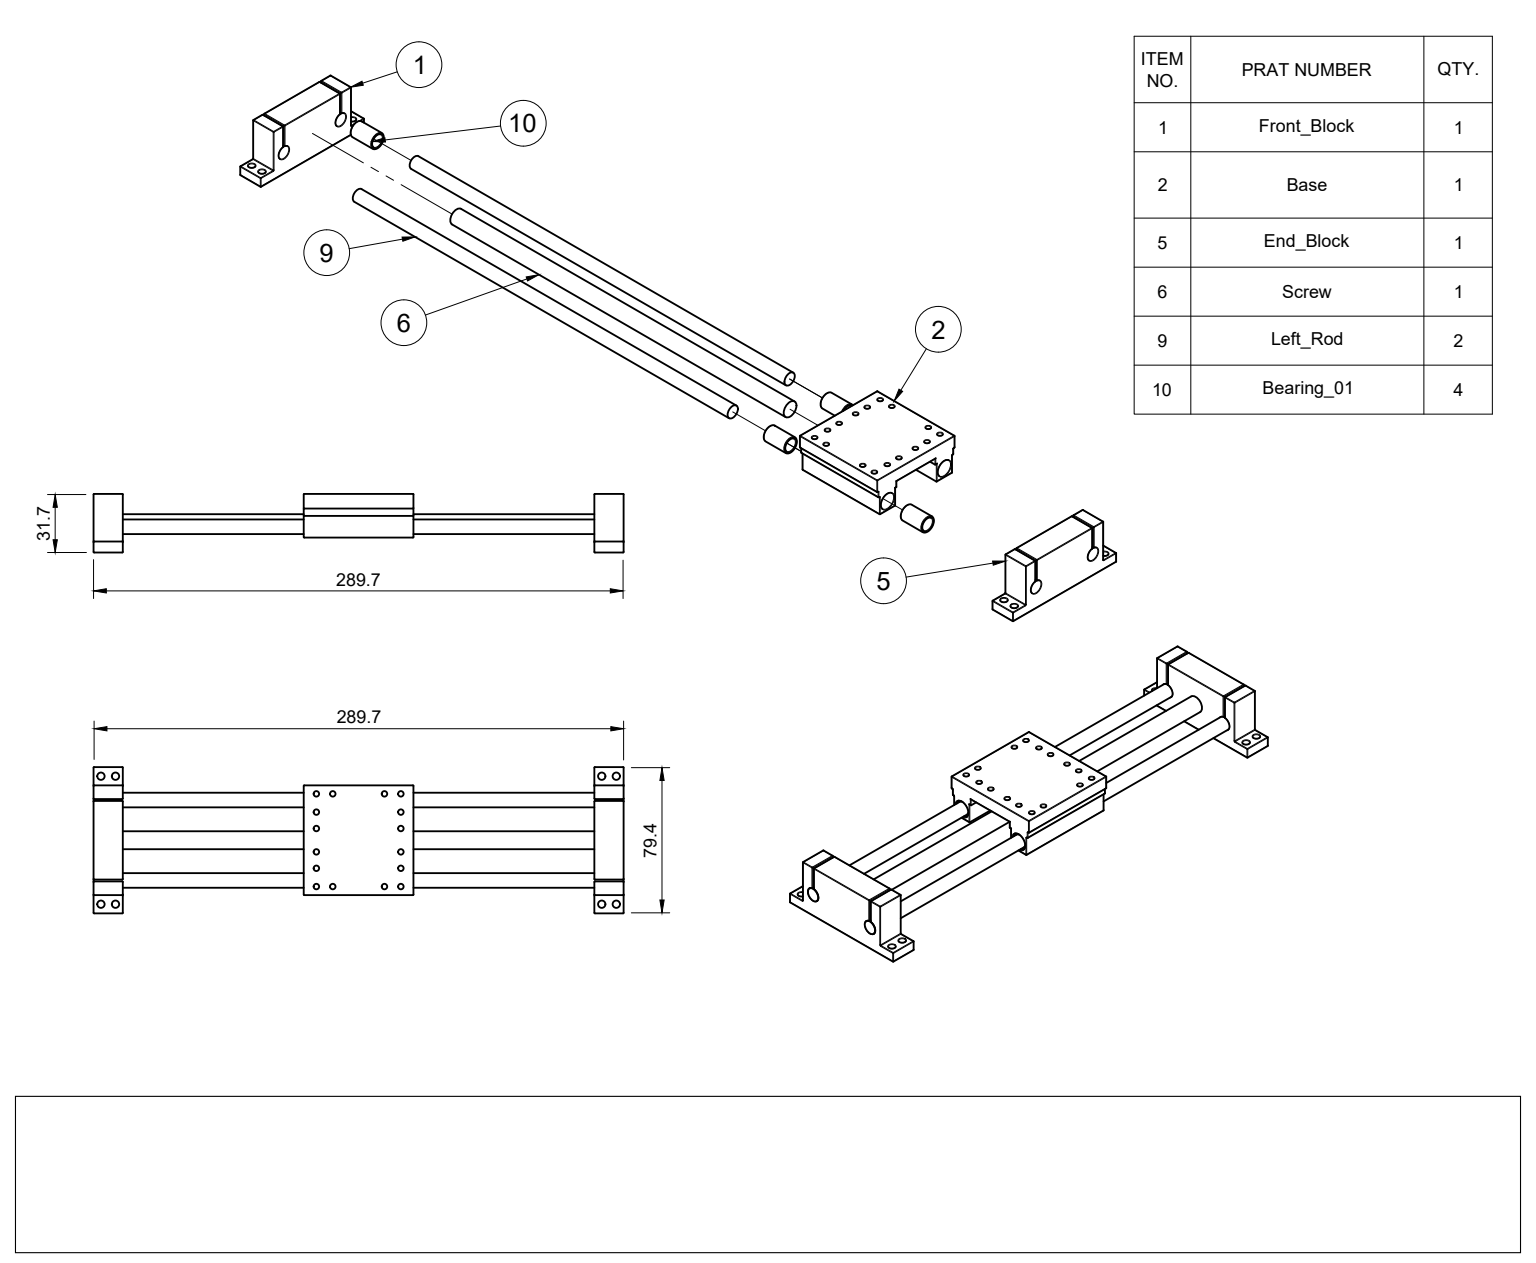
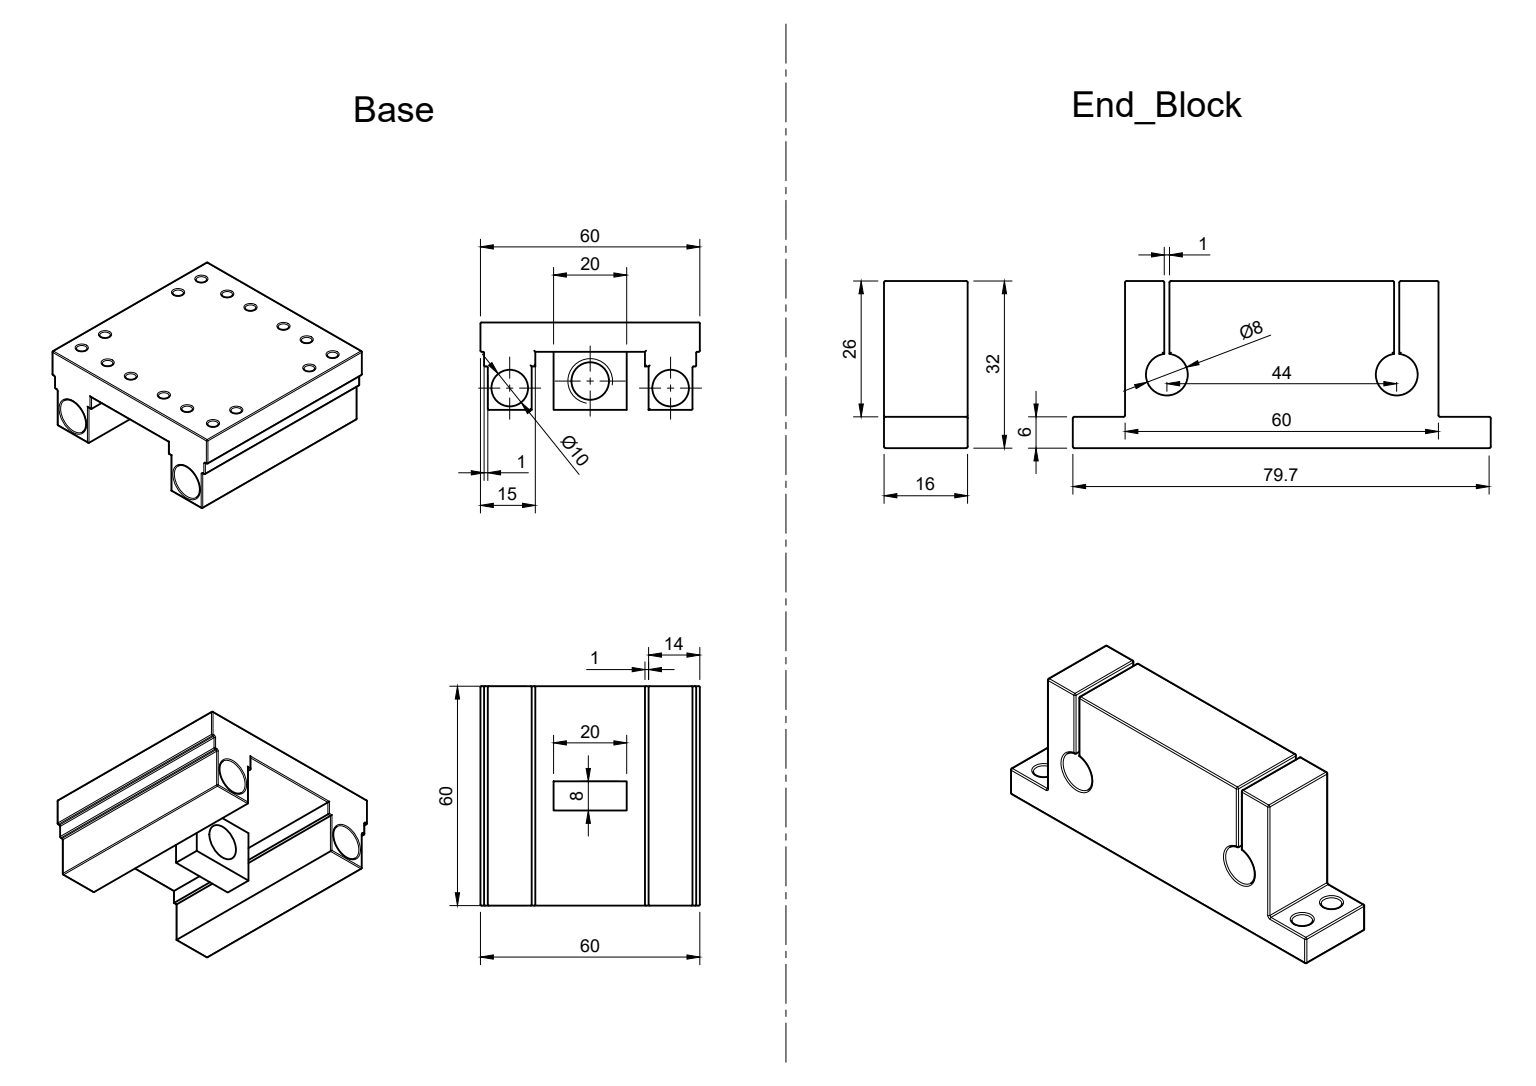
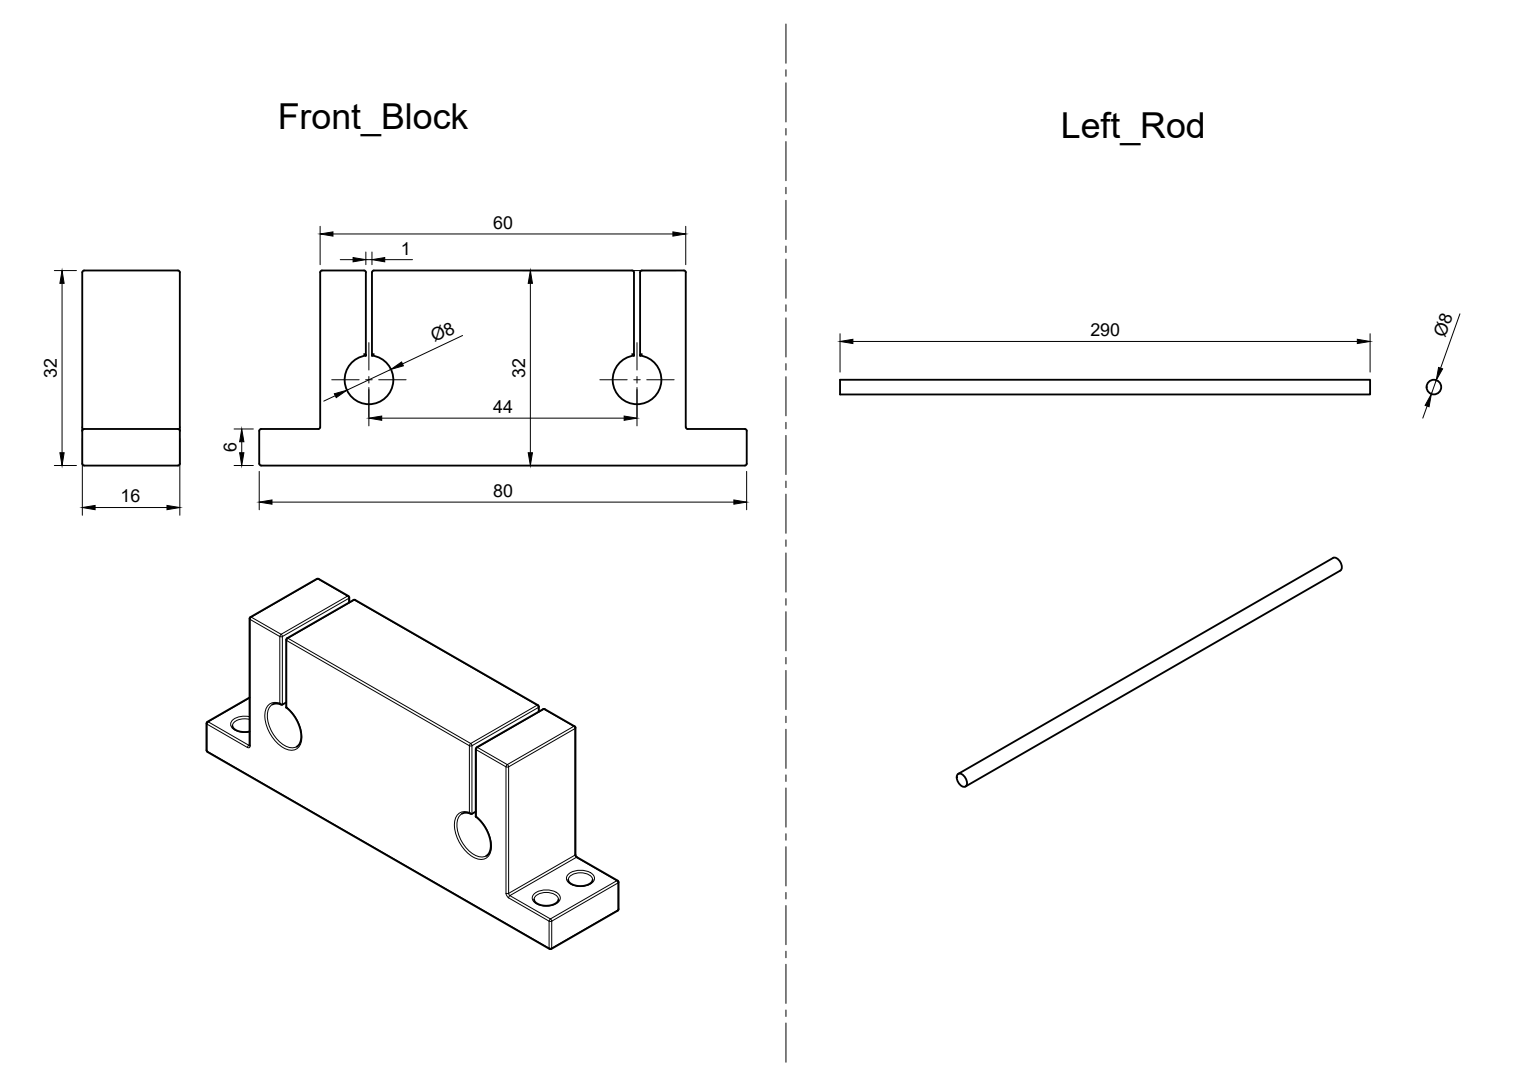
ISO-10303-21;
HEADER;
/* Generated by software containing ST-Developer
 * from STEP Tools, Inc. (www.steptools.com) 
 */

FILE_DESCRIPTION(
/* description */ (''),
/* implementation_level */ '2;1');

FILE_NAME(
/* name */ 'MAS-273',
/* time_stamp */ '2026-10-19T01:30:23+06:00',
/* author */ (''),
/* organization */ (''),
/* preprocessor_version */ 'ST-DEVELOPER v20.2',
/* originating_system */ 'Autodesk Translation Framework v15.15.0.0',
/* authorisation */ '');

FILE_SCHEMA (('AUTOMOTIVE_DESIGN { 1 0 10303 214 3 1 1 }'));
ENDSEC;

DATA;
#10=MECHANICAL_DESIGN_GEOMETRIC_PRESENTATION_REPRESENTATION('',(#87,#88,
#89,#90,#91,#92,#93,#94,#95,#96),#10639);
#11=ITEM_DEFINED_TRANSFORMATION($,$,#5835,#6686);
#12=ITEM_DEFINED_TRANSFORMATION($,$,#6174,#6687);
#13=ITEM_DEFINED_TRANSFORMATION($,$,#6199,#6688);
#14=ITEM_DEFINED_TRANSFORMATION($,$,#6224,#6689);
#15=ITEM_DEFINED_TRANSFORMATION($,$,#6421,#6690);
#16=ITEM_DEFINED_TRANSFORMATION($,$,#6427,#6691);
#17=ITEM_DEFINED_TRANSFORMATION($,$,#6452,#6692);
#18=ITEM_DEFINED_TRANSFORMATION($,$,#6458,#6693);
#19=ITEM_DEFINED_TRANSFORMATION($,$,#6464,#6694);
#20=ITEM_DEFINED_TRANSFORMATION($,$,#6489,#6695);
#21=(
REPRESENTATION_RELATIONSHIP($,$,#10677,#10676)
REPRESENTATION_RELATIONSHIP_WITH_TRANSFORMATION(#11)
SHAPE_REPRESENTATION_RELATIONSHIP()
);
#22=(
REPRESENTATION_RELATIONSHIP($,$,#10678,#10676)
REPRESENTATION_RELATIONSHIP_WITH_TRANSFORMATION(#12)
SHAPE_REPRESENTATION_RELATIONSHIP()
);
#23=(
REPRESENTATION_RELATIONSHIP($,$,#10679,#10676)
REPRESENTATION_RELATIONSHIP_WITH_TRANSFORMATION(#13)
SHAPE_REPRESENTATION_RELATIONSHIP()
);
#24=(
REPRESENTATION_RELATIONSHIP($,$,#10680,#10676)
REPRESENTATION_RELATIONSHIP_WITH_TRANSFORMATION(#14)
SHAPE_REPRESENTATION_RELATIONSHIP()
);
#25=(
REPRESENTATION_RELATIONSHIP($,$,#10681,#10676)
REPRESENTATION_RELATIONSHIP_WITH_TRANSFORMATION(#15)
SHAPE_REPRESENTATION_RELATIONSHIP()
);
#26=(
REPRESENTATION_RELATIONSHIP($,$,#10682,#10676)
REPRESENTATION_RELATIONSHIP_WITH_TRANSFORMATION(#16)
SHAPE_REPRESENTATION_RELATIONSHIP()
);
#27=(
REPRESENTATION_RELATIONSHIP($,$,#10683,#10676)
REPRESENTATION_RELATIONSHIP_WITH_TRANSFORMATION(#17)
SHAPE_REPRESENTATION_RELATIONSHIP()
);
#28=(
REPRESENTATION_RELATIONSHIP($,$,#10684,#10676)
REPRESENTATION_RELATIONSHIP_WITH_TRANSFORMATION(#18)
SHAPE_REPRESENTATION_RELATIONSHIP()
);
#29=(
REPRESENTATION_RELATIONSHIP($,$,#10685,#10676)
REPRESENTATION_RELATIONSHIP_WITH_TRANSFORMATION(#19)
SHAPE_REPRESENTATION_RELATIONSHIP()
);
#30=(
REPRESENTATION_RELATIONSHIP($,$,#10686,#10676)
REPRESENTATION_RELATIONSHIP_WITH_TRANSFORMATION(#20)
SHAPE_REPRESENTATION_RELATIONSHIP()
);
#31=CONTEXT_DEPENDENT_SHAPE_REPRESENTATION(#21,#10666);
#32=CONTEXT_DEPENDENT_SHAPE_REPRESENTATION(#22,#10667);
#33=CONTEXT_DEPENDENT_SHAPE_REPRESENTATION(#23,#10668);
#34=CONTEXT_DEPENDENT_SHAPE_REPRESENTATION(#24,#10669);
#35=CONTEXT_DEPENDENT_SHAPE_REPRESENTATION(#25,#10670);
#36=CONTEXT_DEPENDENT_SHAPE_REPRESENTATION(#26,#10671);
#37=CONTEXT_DEPENDENT_SHAPE_REPRESENTATION(#27,#10672);
#38=CONTEXT_DEPENDENT_SHAPE_REPRESENTATION(#28,#10673);
#39=CONTEXT_DEPENDENT_SHAPE_REPRESENTATION(#29,#10674);
#40=CONTEXT_DEPENDENT_SHAPE_REPRESENTATION(#30,#10675);
#41=NEXT_ASSEMBLY_USAGE_OCCURRENCE('Base:1','Base:1','Base:1',#10688,#10689,
'Base:1');
#42=NEXT_ASSEMBLY_USAGE_OCCURRENCE('Bearing_03:1','Bearing_03:1',
'Bearing_03:1',#10688,#10690,'Bearing_03:1');
#43=NEXT_ASSEMBLY_USAGE_OCCURRENCE('Bearing_04:1','Bearing_04:1',
'Bearing_04:1',#10688,#10691,'Bearing_04:1');
#44=NEXT_ASSEMBLY_USAGE_OCCURRENCE('End_Block:1','End_Block:1',
'End_Block:1',#10688,#10692,'End_Block:1');
#45=NEXT_ASSEMBLY_USAGE_OCCURRENCE('Screw:1','Screw:1','Screw:1',#10688,
#10693,'Screw:1');
#46=NEXT_ASSEMBLY_USAGE_OCCURRENCE('Bearing_02:1','Bearing_02:1',
'Bearing_02:1',#10688,#10694,'Bearing_02:1');
#47=NEXT_ASSEMBLY_USAGE_OCCURRENCE('Left_Rod:1','Left_Rod:1',
'Left_Rod:1',#10688,#10695,'Left_Rod:1');
#48=NEXT_ASSEMBLY_USAGE_OCCURRENCE('Right_Rod:1','Right_Rod:1',
'Right_Rod:1',#10688,#10696,'Right_Rod:1');
#49=NEXT_ASSEMBLY_USAGE_OCCURRENCE('Bearing_01:1','Bearing_01:1',
'Bearing_01:1',#10688,#10697,'Bearing_01:1');
#50=NEXT_ASSEMBLY_USAGE_OCCURRENCE('Front_Block:1','Front_Block:1',
'Front_Block:1',#10688,#10698,'Front_Block:1');
#51=B_SPLINE_CURVE_WITH_KNOTS('',3,(#9730,#9731,#9732,#9733,#9734,#9735,
#9736,#9737,#9738,#9739,#9740,#9741,#9742,#9743),.UNSPECIFIED.,.F.,.F.,
(4,2,2,2,2,2,4),(-0.0546723895048706,-0.0456918425711812,-0.0355825901397237,
-0.0226053755936092,-0.0114630731161328,0.,0.000317608874346033),
 .UNSPECIFIED.);
#52=B_SPLINE_CURVE_WITH_KNOTS('',3,(#9762,#9763,#9764,#9765,#9766,#9767,
#9768,#9769,#9770,#9771,#9772,#9773,#9774,#9775),.UNSPECIFIED.,.F.,.F.,
(4,2,2,2,2,2,4),(-0.0545709206888463,-0.0542557323018554,-0.0428800190516867,
-0.0318226318386046,-0.0189443163854003,-0.00891210636484469,0.),
 .UNSPECIFIED.);
#53=B_SPLINE_CURVE_WITH_KNOTS('',3,(#9781,#9782,#9783,#9784,#9785,#9786,
#9787,#9788,#9789,#9790,#9791,#9792,#9793,#9794),.UNSPECIFIED.,.F.,.F.,
(4,2,2,2,2,2,4),(-0.054570920688858,-0.0542557323018634,-0.0428800190517046,
-0.0318226318386095,-0.0189443163853947,-0.00891210636484256,0.),
 .UNSPECIFIED.);
#54=B_SPLINE_CURVE_WITH_KNOTS('',3,(#9800,#9801,#9802,#9803,#9804,#9805,
#9806,#9807,#9808,#9809,#9810,#9811,#9812,#9813),.UNSPECIFIED.,.F.,.F.,
(4,2,2,2,2,2,4),(-0.0546723899568943,-0.0456918429465685,-0.035582590428848,
-0.0226053757720057,-0.0114630731991726,0.,0.000317608880617367),
 .UNSPECIFIED.);
#55=B_SPLINE_CURVE_WITH_KNOTS('',3,(#9850,#9851,#9852,#9853,#9854,#9855,
#9856,#9857,#9858,#9859,#9860,#9861,#9862,#9863),.UNSPECIFIED.,.F.,.F.,
(4,2,2,2,2,2,4),(-0.0545709206888251,-0.0542557323018344,-0.0428800190516725,
-0.031822631838589,-0.0189443163853906,-0.00891210636484253,0.),
 .UNSPECIFIED.);
#56=B_SPLINE_CURVE_WITH_KNOTS('',3,(#9875,#9876,#9877,#9878,#9879,#9880,
#9881,#9882,#9883,#9884,#9885,#9886,#9887,#9888),.UNSPECIFIED.,.F.,.F.,
(4,2,2,2,2,2,4),(-0.0546723899569042,-0.0456918429465809,-0.0355825904288576,
-0.0226053757720114,-0.0114630731991751,0.,0.000317608880617457),
 .UNSPECIFIED.);
#57=B_SPLINE_CURVE_WITH_KNOTS('',3,(#9897,#9898,#9899,#9900,#9901,#9902,
#9903,#9904,#9905,#9906,#9907,#9908,#9909,#9910),.UNSPECIFIED.,.F.,.F.,
(4,2,2,2,2,2,4),(-0.0546723899569031,-0.0456918429465823,-0.0355825904288603,
-0.0226053757720111,-0.0114630731991739,0.,0.000317608880617373),
 .UNSPECIFIED.);
#58=B_SPLINE_CURVE_WITH_KNOTS('',3,(#9919,#9920,#9921,#9922,#9923,#9924,
#9925,#9926,#9927,#9928,#9929,#9930,#9931,#9932),.UNSPECIFIED.,.F.,.F.,
(4,2,2,2,2,2,4),(-0.0545709206996626,-0.0542557323162056,-0.0428800190513851,
-0.0318226318385961,-0.0189443163854002,-0.00891210636484565,0.),
 .UNSPECIFIED.);
#59=B_SPLINE_CURVE_WITH_KNOTS('',3,(#10339,#10340,#10341,#10342,#10343,
#10344,#10345,#10346,#10347,#10348,#10349,#10350,#10351,#10352),
 .UNSPECIFIED.,.F.,.F.,(4,2,2,2,2,2,4),(-0.0546723895048706,-0.0456918425711812,
-0.0355825901397237,-0.0226053755936092,-0.0114630731161328,0.,0.000317608874346033),
 .UNSPECIFIED.);
#60=B_SPLINE_CURVE_WITH_KNOTS('',3,(#10371,#10372,#10373,#10374,#10375,
#10376,#10377,#10378,#10379,#10380,#10381,#10382,#10383,#10384),
 .UNSPECIFIED.,.F.,.F.,(4,2,2,2,2,2,4),(-0.0545709206888463,-0.0542557323018554,
-0.0428800190516867,-0.0318226318386046,-0.0189443163854003,-0.00891210636484469,
0.),.UNSPECIFIED.);
#61=B_SPLINE_CURVE_WITH_KNOTS('',3,(#10390,#10391,#10392,#10393,#10394,
#10395,#10396,#10397,#10398,#10399,#10400,#10401,#10402,#10403),
 .UNSPECIFIED.,.F.,.F.,(4,2,2,2,2,2,4),(-0.054570920688858,-0.0542557323018634,
-0.0428800190517046,-0.0318226318386095,-0.0189443163853947,-0.00891210636484256,
0.),.UNSPECIFIED.);
#62=B_SPLINE_CURVE_WITH_KNOTS('',3,(#10409,#10410,#10411,#10412,#10413,
#10414,#10415,#10416,#10417,#10418,#10419,#10420,#10421,#10422),
 .UNSPECIFIED.,.F.,.F.,(4,2,2,2,2,2,4),(-0.0546723899568943,-0.0456918429465685,
-0.035582590428848,-0.0226053757720057,-0.0114630731991726,0.,0.000317608880617367),
 .UNSPECIFIED.);
#63=B_SPLINE_CURVE_WITH_KNOTS('',3,(#10459,#10460,#10461,#10462,#10463,
#10464,#10465,#10466,#10467,#10468,#10469,#10470,#10471,#10472),
 .UNSPECIFIED.,.F.,.F.,(4,2,2,2,2,2,4),(-0.0545709206888251,-0.0542557323018344,
-0.0428800190516725,-0.031822631838589,-0.0189443163853906,-0.00891210636484253,
0.),.UNSPECIFIED.);
#64=B_SPLINE_CURVE_WITH_KNOTS('',3,(#10484,#10485,#10486,#10487,#10488,
#10489,#10490,#10491,#10492,#10493,#10494,#10495,#10496,#10497),
 .UNSPECIFIED.,.F.,.F.,(4,2,2,2,2,2,4),(-0.0546723899569042,-0.0456918429465809,
-0.0355825904288576,-0.0226053757720114,-0.0114630731991751,0.,0.000317608880617457),
 .UNSPECIFIED.);
#65=B_SPLINE_CURVE_WITH_KNOTS('',3,(#10506,#10507,#10508,#10509,#10510,
#10511,#10512,#10513,#10514,#10515,#10516,#10517,#10518,#10519),
 .UNSPECIFIED.,.F.,.F.,(4,2,2,2,2,2,4),(-0.0546723899569031,-0.0456918429465823,
-0.0355825904288603,-0.0226053757720111,-0.0114630731991739,0.,0.000317608880617373),
 .UNSPECIFIED.);
#66=B_SPLINE_CURVE_WITH_KNOTS('',3,(#10528,#10529,#10530,#10531,#10532,
#10533,#10534,#10535,#10536,#10537,#10538,#10539,#10540,#10541),
 .UNSPECIFIED.,.F.,.F.,(4,2,2,2,2,2,4),(-0.0545709206996626,-0.0542557323162056,
-0.0428800190513851,-0.0318226318385961,-0.0189443163854002,-0.00891210636484565,
0.),.UNSPECIFIED.);
#67=SHAPE_REPRESENTATION_RELATIONSHIP('SRR','None',#10677,#77);
#68=SHAPE_REPRESENTATION_RELATIONSHIP('SRR','None',#10678,#78);
#69=SHAPE_REPRESENTATION_RELATIONSHIP('SRR','None',#10679,#79);
#70=SHAPE_REPRESENTATION_RELATIONSHIP('SRR','None',#10680,#80);
#71=SHAPE_REPRESENTATION_RELATIONSHIP('SRR','None',#10681,#81);
#72=SHAPE_REPRESENTATION_RELATIONSHIP('SRR','None',#10682,#82);
#73=SHAPE_REPRESENTATION_RELATIONSHIP('SRR','None',#10683,#83);
#74=SHAPE_REPRESENTATION_RELATIONSHIP('SRR','None',#10684,#84);
#75=SHAPE_REPRESENTATION_RELATIONSHIP('SRR','None',#10685,#85);
#76=SHAPE_REPRESENTATION_RELATIONSHIP('SRR','None',#10686,#86);
#77=ADVANCED_BREP_SHAPE_REPRESENTATION('',(#97),#10629);
#78=ADVANCED_BREP_SHAPE_REPRESENTATION('',(#98),#10630);
#79=ADVANCED_BREP_SHAPE_REPRESENTATION('',(#99),#10631);
#80=ADVANCED_BREP_SHAPE_REPRESENTATION('',(#100),#10632);
#81=ADVANCED_BREP_SHAPE_REPRESENTATION('',(#101),#10633);
#82=ADVANCED_BREP_SHAPE_REPRESENTATION('',(#102),#10634);
#83=ADVANCED_BREP_SHAPE_REPRESENTATION('',(#103),#10635);
#84=ADVANCED_BREP_SHAPE_REPRESENTATION('',(#104),#10636);
#85=ADVANCED_BREP_SHAPE_REPRESENTATION('',(#105),#10637);
#86=ADVANCED_BREP_SHAPE_REPRESENTATION('',(#106),#10638);
#87=STYLED_ITEM('',(#10769),#97);
#88=STYLED_ITEM('',(#10790),#98);
#89=STYLED_ITEM('',(#10790),#99);
#90=STYLED_ITEM('',(#10769),#100);
#91=STYLED_ITEM('',(#10797),#101);
#92=STYLED_ITEM('',(#10790),#102);
#93=STYLED_ITEM('',(#10790),#103);
#94=STYLED_ITEM('',(#10790),#104);
#95=STYLED_ITEM('',(#10790),#105);
#96=STYLED_ITEM('',(#10769),#106);
#97=MANIFOLD_SOLID_BREP('Base',#5713);
#98=MANIFOLD_SOLID_BREP('Bearing_03',#5714);
#99=MANIFOLD_SOLID_BREP('Bearing_04',#5715);
#100=MANIFOLD_SOLID_BREP('End_Block',#5716);
#101=MANIFOLD_SOLID_BREP('Screw',#5717);
#102=MANIFOLD_SOLID_BREP('Bearing_02',#5718);
#103=MANIFOLD_SOLID_BREP('Left_Rod',#5719);
#104=MANIFOLD_SOLID_BREP('Right_Rod',#5720);
#105=MANIFOLD_SOLID_BREP('Bearing_01',#5721);
#106=MANIFOLD_SOLID_BREP('Front_Block',#5722);
#107=SPHERICAL_SURFACE('',#5994,0.299999999999998);
#108=SPHERICAL_SURFACE('',#5998,0.3);
#109=SPHERICAL_SURFACE('',#6004,0.299999999999998);
#110=SPHERICAL_SURFACE('',#6014,0.3);
#111=SPHERICAL_SURFACE('',#6030,0.299999999999998);
#112=SPHERICAL_SURFACE('',#6038,0.3);
#113=SPHERICAL_SURFACE('',#6044,0.3);
#114=SPHERICAL_SURFACE('',#6052,0.299999999999994);
#115=SPHERICAL_SURFACE('',#6067,0.299999999999998);
#116=SPHERICAL_SURFACE('',#6075,0.3);
#117=SPHERICAL_SURFACE('',#6081,0.3);
#118=SPHERICAL_SURFACE('',#6085,0.3);
#119=SPHERICAL_SURFACE('',#6089,0.299999999999998);
#120=SPHERICAL_SURFACE('',#6094,0.299999999999998);
#121=SPHERICAL_SURFACE('',#6100,0.299999999999998);
#122=SPHERICAL_SURFACE('',#6104,0.300000000000002);
#123=SPHERICAL_SURFACE('',#6253,0.3);
#124=SPHERICAL_SURFACE('',#6257,0.299999999999994);
#125=SPHERICAL_SURFACE('',#6261,0.300000000000011);
#126=SPHERICAL_SURFACE('',#6266,0.299999999999998);
#127=SPHERICAL_SURFACE('',#6271,0.3);
#128=SPHERICAL_SURFACE('',#6277,0.299999999999994);
#129=SPHERICAL_SURFACE('',#6282,0.3);
#130=SPHERICAL_SURFACE('',#6291,0.3);
#131=SPHERICAL_SURFACE('',#6306,0.299999999999998);
#132=SPHERICAL_SURFACE('',#6316,0.299999999999994);
#133=SPHERICAL_SURFACE('',#6321,0.299999999999994);
#134=SPHERICAL_SURFACE('',#6326,0.3);
#135=SPHERICAL_SURFACE('',#6331,0.299999999999994);
#136=SPHERICAL_SURFACE('',#6337,0.299999999999998);
#137=SPHERICAL_SURFACE('',#6341,0.300000000000002);
#138=SPHERICAL_SURFACE('',#6346,0.3);
#139=SPHERICAL_SURFACE('',#6355,0.3);
#140=SPHERICAL_SURFACE('',#6359,0.3);
#141=SPHERICAL_SURFACE('',#6363,0.3);
#142=SPHERICAL_SURFACE('',#6368,0.299999999999994);
#143=SPHERICAL_SURFACE('',#6518,0.3);
#144=SPHERICAL_SURFACE('',#6522,0.299999999999994);
#145=SPHERICAL_SURFACE('',#6526,0.300000000000011);
#146=SPHERICAL_SURFACE('',#6531,0.299999999999998);
#147=SPHERICAL_SURFACE('',#6536,0.3);
#148=SPHERICAL_SURFACE('',#6542,0.299999999999994);
#149=SPHERICAL_SURFACE('',#6547,0.3);
#150=SPHERICAL_SURFACE('',#6556,0.3);
#151=SPHERICAL_SURFACE('',#6571,0.299999999999998);
#152=SPHERICAL_SURFACE('',#6581,0.299999999999994);
#153=SPHERICAL_SURFACE('',#6586,0.299999999999994);
#154=SPHERICAL_SURFACE('',#6591,0.3);
#155=SPHERICAL_SURFACE('',#6596,0.299999999999994);
#156=SPHERICAL_SURFACE('',#6602,0.299999999999998);
#157=SPHERICAL_SURFACE('',#6606,0.300000000000002);
#158=SPHERICAL_SURFACE('',#6611,0.3);
#159=SPHERICAL_SURFACE('',#6620,0.3);
#160=SPHERICAL_SURFACE('',#6624,0.3);
#161=SPHERICAL_SURFACE('',#6628,0.3);
#162=SPHERICAL_SURFACE('',#6633,0.299999999999994);
#163=ELLIPSE('',#5976,0.42426406871193,0.3);
#164=ELLIPSE('',#5977,0.424264068711927,0.3);
#165=ELLIPSE('',#5979,0.42426406871193,0.3);
#166=ELLIPSE('',#5980,0.424264068711927,0.3);
#167=ELLIPSE('',#5982,0.424264068711929,0.3);
#168=ELLIPSE('',#5984,0.424264068711929,0.3);
#169=ELLIPSE('',#5986,0.424264068711929,0.3);
#170=ELLIPSE('',#5988,0.424264068711929,0.3);
#171=ELLIPSE('',#5990,0.424264068711929,0.3);
#172=ELLIPSE('',#5991,0.424264068711929,0.3);
#173=ELLIPSE('',#5993,0.424264068711929,0.3);
#174=ELLIPSE('',#6009,0.424264068711929,0.3);
#175=ELLIPSE('',#6019,0.424264068711929,0.3);
#176=ELLIPSE('',#6131,0.424264068711929,0.3);
#177=ELLIPSE('',#6134,0.424264068711929,0.3);
#178=ELLIPSE('',#6137,0.424264068711929,0.3);
#179=TOROIDAL_SURFACE('',#5844,5.3,0.3);
#180=TOROIDAL_SURFACE('',#5858,5.3,0.3);
#181=TOROIDAL_SURFACE('',#5865,5.3,0.3);
#182=TOROIDAL_SURFACE('',#5874,5.3,0.3);
#183=TOROIDAL_SURFACE('',#5876,1.8,0.3);
#184=TOROIDAL_SURFACE('',#5898,1.8,0.3);
#185=TOROIDAL_SURFACE('',#5903,1.8,0.3);
#186=TOROIDAL_SURFACE('',#5908,1.8,0.3);
#187=TOROIDAL_SURFACE('',#5913,1.8,0.3);
#188=TOROIDAL_SURFACE('',#5918,1.8,0.3);
#189=TOROIDAL_SURFACE('',#5923,1.8,0.3);
#190=TOROIDAL_SURFACE('',#5928,1.8,0.3);
#191=TOROIDAL_SURFACE('',#5934,1.8,0.3);
#192=TOROIDAL_SURFACE('',#5939,1.8,0.3);
#193=TOROIDAL_SURFACE('',#5945,1.8,0.3);
#194=TOROIDAL_SURFACE('',#5950,1.8,0.3);
#195=TOROIDAL_SURFACE('',#5955,1.8,0.3);
#196=TOROIDAL_SURFACE('',#5960,1.8,0.3);
#197=TOROIDAL_SURFACE('',#5965,1.8,0.3);
#198=TOROIDAL_SURFACE('',#5970,1.8,0.3);
#199=TOROIDAL_SURFACE('',#6010,0.599999999999996,0.299999999999998);
#200=TOROIDAL_SURFACE('',#6021,0.600000000000001,0.3);
#201=TOROIDAL_SURFACE('',#6026,0.599999999999996,0.299999999999998);
#202=TOROIDAL_SURFACE('',#6034,0.599999999999996,0.299999999999998);
#203=TOROIDAL_SURFACE('',#6048,0.600000000000001,0.299999999999998);
#204=TOROIDAL_SURFACE('',#6057,0.600000000000001,0.3);
#205=TOROIDAL_SURFACE('',#6062,0.600000000000001,0.3);
#206=TOROIDAL_SURFACE('',#6071,0.599999999999996,0.299999999999998);
#207=TOROIDAL_SURFACE('',#6175,4.3,0.3);
#208=TOROIDAL_SURFACE('',#6185,4.7,0.3);
#209=TOROIDAL_SURFACE('',#6192,4.3,0.3);
#210=TOROIDAL_SURFACE('',#6197,4.7,0.3);
#211=TOROIDAL_SURFACE('',#6200,4.3,0.3);
#212=TOROIDAL_SURFACE('',#6210,4.7,0.3);
#213=TOROIDAL_SURFACE('',#6217,4.3,0.3);
#214=TOROIDAL_SURFACE('',#6222,4.7,0.3);
#215=TOROIDAL_SURFACE('',#6225,2.29999999999999,0.3);
#216=TOROIDAL_SURFACE('',#6233,2.29999999999999,0.3);
#217=TOROIDAL_SURFACE('',#6238,2.29999999999999,0.3);
#218=TOROIDAL_SURFACE('',#6247,2.29999999999999,0.3);
#219=TOROIDAL_SURFACE('',#6286,0.600000000000001,0.3);
#220=TOROIDAL_SURFACE('',#6296,0.600000000000001,0.299999999999994);
#221=TOROIDAL_SURFACE('',#6301,0.600000000000001,0.299999999999976);
#222=TOROIDAL_SURFACE('',#6311,0.600000000000001,0.3);
#223=TOROIDAL_SURFACE('',#6378,4.3,0.3);
#224=TOROIDAL_SURFACE('',#6382,4.3,0.3);
#225=TOROIDAL_SURFACE('',#6385,4.3,0.3);
#226=TOROIDAL_SURFACE('',#6388,4.3,0.3);
#227=TOROIDAL_SURFACE('',#6428,4.3,0.3);
#228=TOROIDAL_SURFACE('',#6438,4.7,0.3);
#229=TOROIDAL_SURFACE('',#6445,4.3,0.3);
#230=TOROIDAL_SURFACE('',#6450,4.7,0.3);
#231=TOROIDAL_SURFACE('',#6465,4.3,0.3);
#232=TOROIDAL_SURFACE('',#6475,4.7,0.3);
#233=TOROIDAL_SURFACE('',#6482,4.3,0.3);
#234=TOROIDAL_SURFACE('',#6487,4.7,0.3);
#235=TOROIDAL_SURFACE('',#6490,2.29999999999999,0.3);
#236=TOROIDAL_SURFACE('',#6498,2.29999999999999,0.3);
#237=TOROIDAL_SURFACE('',#6503,2.29999999999999,0.3);
#238=TOROIDAL_SURFACE('',#6512,2.29999999999999,0.3);
#239=TOROIDAL_SURFACE('',#6551,0.600000000000001,0.3);
#240=TOROIDAL_SURFACE('',#6561,0.600000000000001,0.299999999999994);
#241=TOROIDAL_SURFACE('',#6566,0.600000000000001,0.299999999999976);
#242=TOROIDAL_SURFACE('',#6576,0.600000000000001,0.3);
#243=TOROIDAL_SURFACE('',#6643,4.3,0.3);
#244=TOROIDAL_SURFACE('',#6647,4.3,0.3);
#245=TOROIDAL_SURFACE('',#6650,4.3,0.3);
#246=TOROIDAL_SURFACE('',#6653,4.3,0.3);
#247=FACE_BOUND('',#773,.T.);
#248=FACE_BOUND('',#776,.T.);
#249=FACE_BOUND('',#780,.T.);
#250=FACE_BOUND('',#781,.T.);
#251=FACE_BOUND('',#787,.T.);
#252=FACE_BOUND('',#788,.T.);
#253=FACE_BOUND('',#792,.T.);
#254=FACE_BOUND('',#793,.T.);
#255=FACE_BOUND('',#794,.T.);
#256=FACE_BOUND('',#795,.T.);
#257=FACE_BOUND('',#796,.T.);
#258=FACE_BOUND('',#797,.T.);
#259=FACE_BOUND('',#798,.T.);
#260=FACE_BOUND('',#799,.T.);
#261=FACE_BOUND('',#800,.T.);
#262=FACE_BOUND('',#801,.T.);
#263=FACE_BOUND('',#802,.T.);
#264=FACE_BOUND('',#803,.T.);
#265=FACE_BOUND('',#804,.T.);
#266=FACE_BOUND('',#805,.T.);
#267=FACE_BOUND('',#806,.T.);
#268=FACE_BOUND('',#807,.T.);
#269=FACE_BOUND('',#919,.T.);
#270=FACE_BOUND('',#953,.T.);
#271=FACE_BOUND('',#959,.T.);
#272=FACE_BOUND('',#963,.T.);
#273=FACE_BOUND('',#969,.T.);
#274=FACE_BOUND('',#973,.T.);
#275=FACE_BOUND('',#974,.T.);
#276=FACE_BOUND('',#980,.T.);
#277=FACE_BOUND('',#981,.T.);
#278=FACE_BOUND('',#1058,.T.);
#279=FACE_BOUND('',#1059,.T.);
#280=FACE_BOUND('',#1060,.T.);
#281=FACE_BOUND('',#1061,.T.);
#282=FACE_BOUND('',#1078,.T.);
#283=FACE_BOUND('',#1084,.T.);
#284=FACE_BOUND('',#1094,.T.);
#285=FACE_BOUND('',#1100,.T.);
#286=FACE_BOUND('',#1104,.T.);
#287=FACE_BOUND('',#1105,.T.);
#288=FACE_BOUND('',#1111,.T.);
#289=FACE_BOUND('',#1112,.T.);
#290=FACE_BOUND('',#1189,.T.);
#291=FACE_BOUND('',#1190,.T.);
#292=FACE_BOUND('',#1191,.T.);
#293=FACE_BOUND('',#1192,.T.);
#294=PLANE('',#5839);
#295=PLANE('',#5840);
#296=PLANE('',#5841);
#297=PLANE('',#5842);
#298=PLANE('',#5843);
#299=PLANE('',#5849);
#300=PLANE('',#5868);
#301=PLANE('',#5880);
#302=PLANE('',#6139);
#303=PLANE('',#6140);
#304=PLANE('',#6141);
#305=PLANE('',#6142);
#306=PLANE('',#6143);
#307=PLANE('',#6144);
#308=PLANE('',#6145);
#309=PLANE('',#6146);
#310=PLANE('',#6147);
#311=PLANE('',#6148);
#312=PLANE('',#6149);
#313=PLANE('',#6150);
#314=PLANE('',#6151);
#315=PLANE('',#6152);
#316=PLANE('',#6153);
#317=PLANE('',#6154);
#318=PLANE('',#6155);
#319=PLANE('',#6156);
#320=PLANE('',#6157);
#321=PLANE('',#6158);
#322=PLANE('',#6159);
#323=PLANE('',#6160);
#324=PLANE('',#6161);
#325=PLANE('',#6162);
#326=PLANE('',#6163);
#327=PLANE('',#6164);
#328=PLANE('',#6165);
#329=PLANE('',#6166);
#330=PLANE('',#6167);
#331=PLANE('',#6168);
#332=PLANE('',#6169);
#333=PLANE('',#6170);
#334=PLANE('',#6171);
#335=PLANE('',#6172);
#336=PLANE('',#6173);
#337=PLANE('',#6180);
#338=PLANE('',#6195);
#339=PLANE('',#6205);
#340=PLANE('',#6220);
#341=PLANE('',#6229);
#342=PLANE('',#6243);
#343=PLANE('',#6405);
#344=PLANE('',#6408);
#345=PLANE('',#6409);
#346=PLANE('',#6410);
#347=PLANE('',#6411);
#348=PLANE('',#6412);
#349=PLANE('',#6413);
#350=PLANE('',#6414);
#351=PLANE('',#6415);
#352=PLANE('',#6416);
#353=PLANE('',#6417);
#354=PLANE('',#6418);
#355=PLANE('',#6419);
#356=PLANE('',#6420);
#357=PLANE('',#6422);
#358=PLANE('',#6426);
#359=PLANE('',#6433);
#360=PLANE('',#6448);
#361=PLANE('',#6453);
#362=PLANE('',#6457);
#363=PLANE('',#6459);
#364=PLANE('',#6463);
#365=PLANE('',#6470);
#366=PLANE('',#6485);
#367=PLANE('',#6494);
#368=PLANE('',#6508);
#369=PLANE('',#6670);
#370=PLANE('',#6673);
#371=PLANE('',#6674);
#372=PLANE('',#6675);
#373=PLANE('',#6676);
#374=PLANE('',#6677);
#375=PLANE('',#6678);
#376=PLANE('',#6679);
#377=PLANE('',#6680);
#378=PLANE('',#6681);
#379=PLANE('',#6682);
#380=PLANE('',#6683);
#381=PLANE('',#6684);
#382=PLANE('',#6685);
#383=FACE_OUTER_BOUND('',#770,.T.);
#384=FACE_OUTER_BOUND('',#771,.T.);
#385=FACE_OUTER_BOUND('',#772,.T.);
#386=FACE_OUTER_BOUND('',#774,.T.);
#387=FACE_OUTER_BOUND('',#775,.T.);
#388=FACE_OUTER_BOUND('',#777,.T.);
#389=FACE_OUTER_BOUND('',#778,.T.);
#390=FACE_OUTER_BOUND('',#779,.T.);
#391=FACE_OUTER_BOUND('',#782,.T.);
#392=FACE_OUTER_BOUND('',#783,.T.);
#393=FACE_OUTER_BOUND('',#784,.T.);
#394=FACE_OUTER_BOUND('',#785,.T.);
#395=FACE_OUTER_BOUND('',#786,.T.);
#396=FACE_OUTER_BOUND('',#789,.T.);
#397=FACE_OUTER_BOUND('',#790,.T.);
#398=FACE_OUTER_BOUND('',#791,.T.);
#399=FACE_OUTER_BOUND('',#808,.T.);
#400=FACE_OUTER_BOUND('',#809,.T.);
#401=FACE_OUTER_BOUND('',#810,.T.);
#402=FACE_OUTER_BOUND('',#811,.T.);
#403=FACE_OUTER_BOUND('',#812,.T.);
#404=FACE_OUTER_BOUND('',#813,.T.);
#405=FACE_OUTER_BOUND('',#814,.T.);
#406=FACE_OUTER_BOUND('',#815,.T.);
#407=FACE_OUTER_BOUND('',#816,.T.);
#408=FACE_OUTER_BOUND('',#817,.T.);
#409=FACE_OUTER_BOUND('',#818,.T.);
#410=FACE_OUTER_BOUND('',#819,.T.);
#411=FACE_OUTER_BOUND('',#820,.T.);
#412=FACE_OUTER_BOUND('',#821,.T.);
#413=FACE_OUTER_BOUND('',#822,.T.);
#414=FACE_OUTER_BOUND('',#823,.T.);
#415=FACE_OUTER_BOUND('',#824,.T.);
#416=FACE_OUTER_BOUND('',#825,.T.);
#417=FACE_OUTER_BOUND('',#826,.T.);
#418=FACE_OUTER_BOUND('',#827,.T.);
#419=FACE_OUTER_BOUND('',#828,.T.);
#420=FACE_OUTER_BOUND('',#829,.T.);
#421=FACE_OUTER_BOUND('',#830,.T.);
#422=FACE_OUTER_BOUND('',#831,.T.);
#423=FACE_OUTER_BOUND('',#832,.T.);
#424=FACE_OUTER_BOUND('',#833,.T.);
#425=FACE_OUTER_BOUND('',#834,.T.);
#426=FACE_OUTER_BOUND('',#835,.T.);
#427=FACE_OUTER_BOUND('',#836,.T.);
#428=FACE_OUTER_BOUND('',#837,.T.);
#429=FACE_OUTER_BOUND('',#838,.T.);
#430=FACE_OUTER_BOUND('',#839,.T.);
#431=FACE_OUTER_BOUND('',#840,.T.);
#432=FACE_OUTER_BOUND('',#841,.T.);
#433=FACE_OUTER_BOUND('',#842,.T.);
#434=FACE_OUTER_BOUND('',#843,.T.);
#435=FACE_OUTER_BOUND('',#844,.T.);
#436=FACE_OUTER_BOUND('',#845,.T.);
#437=FACE_OUTER_BOUND('',#846,.T.);
#438=FACE_OUTER_BOUND('',#847,.T.);
#439=FACE_OUTER_BOUND('',#848,.T.);
#440=FACE_OUTER_BOUND('',#849,.T.);
#441=FACE_OUTER_BOUND('',#850,.T.);
#442=FACE_OUTER_BOUND('',#851,.T.);
#443=FACE_OUTER_BOUND('',#852,.T.);
#444=FACE_OUTER_BOUND('',#853,.T.);
#445=FACE_OUTER_BOUND('',#854,.T.);
#446=FACE_OUTER_BOUND('',#855,.T.);
#447=FACE_OUTER_BOUND('',#856,.T.);
#448=FACE_OUTER_BOUND('',#857,.T.);
#449=FACE_OUTER_BOUND('',#858,.T.);
#450=FACE_OUTER_BOUND('',#859,.T.);
#451=FACE_OUTER_BOUND('',#860,.T.);
#452=FACE_OUTER_BOUND('',#861,.T.);
#453=FACE_OUTER_BOUND('',#862,.T.);
#454=FACE_OUTER_BOUND('',#863,.T.);
#455=FACE_OUTER_BOUND('',#864,.T.);
#456=FACE_OUTER_BOUND('',#865,.T.);
#457=FACE_OUTER_BOUND('',#866,.T.);
#458=FACE_OUTER_BOUND('',#867,.T.);
#459=FACE_OUTER_BOUND('',#868,.T.);
#460=FACE_OUTER_BOUND('',#869,.T.);
#461=FACE_OUTER_BOUND('',#870,.T.);
#462=FACE_OUTER_BOUND('',#871,.T.);
#463=FACE_OUTER_BOUND('',#872,.T.);
#464=FACE_OUTER_BOUND('',#873,.T.);
#465=FACE_OUTER_BOUND('',#874,.T.);
#466=FACE_OUTER_BOUND('',#875,.T.);
#467=FACE_OUTER_BOUND('',#876,.T.);
#468=FACE_OUTER_BOUND('',#877,.T.);
#469=FACE_OUTER_BOUND('',#878,.T.);
#470=FACE_OUTER_BOUND('',#879,.T.);
#471=FACE_OUTER_BOUND('',#880,.T.);
#472=FACE_OUTER_BOUND('',#881,.T.);
#473=FACE_OUTER_BOUND('',#882,.T.);
#474=FACE_OUTER_BOUND('',#883,.T.);
#475=FACE_OUTER_BOUND('',#884,.T.);
#476=FACE_OUTER_BOUND('',#885,.T.);
#477=FACE_OUTER_BOUND('',#886,.T.);
#478=FACE_OUTER_BOUND('',#887,.T.);
#479=FACE_OUTER_BOUND('',#888,.T.);
#480=FACE_OUTER_BOUND('',#889,.T.);
#481=FACE_OUTER_BOUND('',#890,.T.);
#482=FACE_OUTER_BOUND('',#891,.T.);
#483=FACE_OUTER_BOUND('',#892,.T.);
#484=FACE_OUTER_BOUND('',#893,.T.);
#485=FACE_OUTER_BOUND('',#894,.T.);
#486=FACE_OUTER_BOUND('',#895,.T.);
#487=FACE_OUTER_BOUND('',#896,.T.);
#488=FACE_OUTER_BOUND('',#897,.T.);
#489=FACE_OUTER_BOUND('',#898,.T.);
#490=FACE_OUTER_BOUND('',#899,.T.);
#491=FACE_OUTER_BOUND('',#900,.T.);
#492=FACE_OUTER_BOUND('',#901,.T.);
#493=FACE_OUTER_BOUND('',#902,.T.);
#494=FACE_OUTER_BOUND('',#903,.T.);
#495=FACE_OUTER_BOUND('',#904,.T.);
#496=FACE_OUTER_BOUND('',#905,.T.);
#497=FACE_OUTER_BOUND('',#906,.T.);
#498=FACE_OUTER_BOUND('',#907,.T.);
#499=FACE_OUTER_BOUND('',#908,.T.);
#500=FACE_OUTER_BOUND('',#909,.T.);
#501=FACE_OUTER_BOUND('',#910,.T.);
#502=FACE_OUTER_BOUND('',#911,.T.);
#503=FACE_OUTER_BOUND('',#912,.T.);
#504=FACE_OUTER_BOUND('',#913,.T.);
#505=FACE_OUTER_BOUND('',#914,.T.);
#506=FACE_OUTER_BOUND('',#915,.T.);
#507=FACE_OUTER_BOUND('',#916,.T.);
#508=FACE_OUTER_BOUND('',#917,.T.);
#509=FACE_OUTER_BOUND('',#918,.T.);
#510=FACE_OUTER_BOUND('',#920,.T.);
#511=FACE_OUTER_BOUND('',#921,.T.);
#512=FACE_OUTER_BOUND('',#922,.T.);
#513=FACE_OUTER_BOUND('',#923,.T.);
#514=FACE_OUTER_BOUND('',#924,.T.);
#515=FACE_OUTER_BOUND('',#925,.T.);
#516=FACE_OUTER_BOUND('',#926,.T.);
#517=FACE_OUTER_BOUND('',#927,.T.);
#518=FACE_OUTER_BOUND('',#928,.T.);
#519=FACE_OUTER_BOUND('',#929,.T.);
#520=FACE_OUTER_BOUND('',#930,.T.);
#521=FACE_OUTER_BOUND('',#931,.T.);
#522=FACE_OUTER_BOUND('',#932,.T.);
#523=FACE_OUTER_BOUND('',#933,.T.);
#524=FACE_OUTER_BOUND('',#934,.T.);
#525=FACE_OUTER_BOUND('',#935,.T.);
#526=FACE_OUTER_BOUND('',#936,.T.);
#527=FACE_OUTER_BOUND('',#937,.T.);
#528=FACE_OUTER_BOUND('',#938,.T.);
#529=FACE_OUTER_BOUND('',#939,.T.);
#530=FACE_OUTER_BOUND('',#940,.T.);
#531=FACE_OUTER_BOUND('',#941,.T.);
#532=FACE_OUTER_BOUND('',#942,.T.);
#533=FACE_OUTER_BOUND('',#943,.T.);
#534=FACE_OUTER_BOUND('',#944,.T.);
#535=FACE_OUTER_BOUND('',#945,.T.);
#536=FACE_OUTER_BOUND('',#946,.T.);
#537=FACE_OUTER_BOUND('',#947,.T.);
#538=FACE_OUTER_BOUND('',#948,.T.);
#539=FACE_OUTER_BOUND('',#949,.T.);
#540=FACE_OUTER_BOUND('',#950,.T.);
#541=FACE_OUTER_BOUND('',#951,.T.);
#542=FACE_OUTER_BOUND('',#952,.T.);
#543=FACE_OUTER_BOUND('',#954,.T.);
#544=FACE_OUTER_BOUND('',#955,.T.);
#545=FACE_OUTER_BOUND('',#956,.T.);
#546=FACE_OUTER_BOUND('',#957,.T.);
#547=FACE_OUTER_BOUND('',#958,.T.);
#548=FACE_OUTER_BOUND('',#960,.T.);
#549=FACE_OUTER_BOUND('',#961,.T.);
#550=FACE_OUTER_BOUND('',#962,.T.);
#551=FACE_OUTER_BOUND('',#964,.T.);
#552=FACE_OUTER_BOUND('',#965,.T.);
#553=FACE_OUTER_BOUND('',#966,.T.);
#554=FACE_OUTER_BOUND('',#967,.T.);
#555=FACE_OUTER_BOUND('',#968,.T.);
#556=FACE_OUTER_BOUND('',#970,.T.);
#557=FACE_OUTER_BOUND('',#971,.T.);
#558=FACE_OUTER_BOUND('',#972,.T.);
#559=FACE_OUTER_BOUND('',#975,.T.);
#560=FACE_OUTER_BOUND('',#976,.T.);
#561=FACE_OUTER_BOUND('',#977,.T.);
#562=FACE_OUTER_BOUND('',#978,.T.);
#563=FACE_OUTER_BOUND('',#979,.T.);
#564=FACE_OUTER_BOUND('',#982,.T.);
#565=FACE_OUTER_BOUND('',#983,.T.);
#566=FACE_OUTER_BOUND('',#984,.T.);
#567=FACE_OUTER_BOUND('',#985,.T.);
#568=FACE_OUTER_BOUND('',#986,.T.);
#569=FACE_OUTER_BOUND('',#987,.T.);
#570=FACE_OUTER_BOUND('',#988,.T.);
#571=FACE_OUTER_BOUND('',#989,.T.);
#572=FACE_OUTER_BOUND('',#990,.T.);
#573=FACE_OUTER_BOUND('',#991,.T.);
#574=FACE_OUTER_BOUND('',#992,.T.);
#575=FACE_OUTER_BOUND('',#993,.T.);
#576=FACE_OUTER_BOUND('',#994,.T.);
#577=FACE_OUTER_BOUND('',#995,.T.);
#578=FACE_OUTER_BOUND('',#996,.T.);
#579=FACE_OUTER_BOUND('',#997,.T.);
#580=FACE_OUTER_BOUND('',#998,.T.);
#581=FACE_OUTER_BOUND('',#999,.T.);
#582=FACE_OUTER_BOUND('',#1000,.T.);
#583=FACE_OUTER_BOUND('',#1001,.T.);
#584=FACE_OUTER_BOUND('',#1002,.T.);
#585=FACE_OUTER_BOUND('',#1003,.T.);
#586=FACE_OUTER_BOUND('',#1004,.T.);
#587=FACE_OUTER_BOUND('',#1005,.T.);
#588=FACE_OUTER_BOUND('',#1006,.T.);
#589=FACE_OUTER_BOUND('',#1007,.T.);
#590=FACE_OUTER_BOUND('',#1008,.T.);
#591=FACE_OUTER_BOUND('',#1009,.T.);
#592=FACE_OUTER_BOUND('',#1010,.T.);
#593=FACE_OUTER_BOUND('',#1011,.T.);
#594=FACE_OUTER_BOUND('',#1012,.T.);
#595=FACE_OUTER_BOUND('',#1013,.T.);
#596=FACE_OUTER_BOUND('',#1014,.T.);
#597=FACE_OUTER_BOUND('',#1015,.T.);
#598=FACE_OUTER_BOUND('',#1016,.T.);
#599=FACE_OUTER_BOUND('',#1017,.T.);
#600=FACE_OUTER_BOUND('',#1018,.T.);
#601=FACE_OUTER_BOUND('',#1019,.T.);
#602=FACE_OUTER_BOUND('',#1020,.T.);
#603=FACE_OUTER_BOUND('',#1021,.T.);
#604=FACE_OUTER_BOUND('',#1022,.T.);
#605=FACE_OUTER_BOUND('',#1023,.T.);
#606=FACE_OUTER_BOUND('',#1024,.T.);
#607=FACE_OUTER_BOUND('',#1025,.T.);
#608=FACE_OUTER_BOUND('',#1026,.T.);
#609=FACE_OUTER_BOUND('',#1027,.T.);
#610=FACE_OUTER_BOUND('',#1028,.T.);
#611=FACE_OUTER_BOUND('',#1029,.T.);
#612=FACE_OUTER_BOUND('',#1030,.T.);
#613=FACE_OUTER_BOUND('',#1031,.T.);
#614=FACE_OUTER_BOUND('',#1032,.T.);
#615=FACE_OUTER_BOUND('',#1033,.T.);
#616=FACE_OUTER_BOUND('',#1034,.T.);
#617=FACE_OUTER_BOUND('',#1035,.T.);
#618=FACE_OUTER_BOUND('',#1036,.T.);
#619=FACE_OUTER_BOUND('',#1037,.T.);
#620=FACE_OUTER_BOUND('',#1038,.T.);
#621=FACE_OUTER_BOUND('',#1039,.T.);
#622=FACE_OUTER_BOUND('',#1040,.T.);
#623=FACE_OUTER_BOUND('',#1041,.T.);
#624=FACE_OUTER_BOUND('',#1042,.T.);
#625=FACE_OUTER_BOUND('',#1043,.T.);
#626=FACE_OUTER_BOUND('',#1044,.T.);
#627=FACE_OUTER_BOUND('',#1045,.T.);
#628=FACE_OUTER_BOUND('',#1046,.T.);
#629=FACE_OUTER_BOUND('',#1047,.T.);
#630=FACE_OUTER_BOUND('',#1048,.T.);
#631=FACE_OUTER_BOUND('',#1049,.T.);
#632=FACE_OUTER_BOUND('',#1050,.T.);
#633=FACE_OUTER_BOUND('',#1051,.T.);
#634=FACE_OUTER_BOUND('',#1052,.T.);
#635=FACE_OUTER_BOUND('',#1053,.T.);
#636=FACE_OUTER_BOUND('',#1054,.T.);
#637=FACE_OUTER_BOUND('',#1055,.T.);
#638=FACE_OUTER_BOUND('',#1056,.T.);
#639=FACE_OUTER_BOUND('',#1057,.T.);
#640=FACE_OUTER_BOUND('',#1062,.T.);
#641=FACE_OUTER_BOUND('',#1063,.T.);
#642=FACE_OUTER_BOUND('',#1064,.T.);
#643=FACE_OUTER_BOUND('',#1065,.T.);
#644=FACE_OUTER_BOUND('',#1066,.T.);
#645=FACE_OUTER_BOUND('',#1067,.T.);
#646=FACE_OUTER_BOUND('',#1068,.T.);
#647=FACE_OUTER_BOUND('',#1069,.T.);
#648=FACE_OUTER_BOUND('',#1070,.T.);
#649=FACE_OUTER_BOUND('',#1071,.T.);
#650=FACE_OUTER_BOUND('',#1072,.T.);
#651=FACE_OUTER_BOUND('',#1073,.T.);
#652=FACE_OUTER_BOUND('',#1074,.T.);
#653=FACE_OUTER_BOUND('',#1075,.T.);
#654=FACE_OUTER_BOUND('',#1076,.T.);
#655=FACE_OUTER_BOUND('',#1077,.T.);
#656=FACE_OUTER_BOUND('',#1079,.T.);
#657=FACE_OUTER_BOUND('',#1080,.T.);
#658=FACE_OUTER_BOUND('',#1081,.T.);
#659=FACE_OUTER_BOUND('',#1082,.T.);
#660=FACE_OUTER_BOUND('',#1083,.T.);
#661=FACE_OUTER_BOUND('',#1085,.T.);
#662=FACE_OUTER_BOUND('',#1086,.T.);
#663=FACE_OUTER_BOUND('',#1087,.T.);
#664=FACE_OUTER_BOUND('',#1088,.T.);
#665=FACE_OUTER_BOUND('',#1089,.T.);
#666=FACE_OUTER_BOUND('',#1090,.T.);
#667=FACE_OUTER_BOUND('',#1091,.T.);
#668=FACE_OUTER_BOUND('',#1092,.T.);
#669=FACE_OUTER_BOUND('',#1093,.T.);
#670=FACE_OUTER_BOUND('',#1095,.T.);
#671=FACE_OUTER_BOUND('',#1096,.T.);
#672=FACE_OUTER_BOUND('',#1097,.T.);
#673=FACE_OUTER_BOUND('',#1098,.T.);
#674=FACE_OUTER_BOUND('',#1099,.T.);
#675=FACE_OUTER_BOUND('',#1101,.T.);
#676=FACE_OUTER_BOUND('',#1102,.T.);
#677=FACE_OUTER_BOUND('',#1103,.T.);
#678=FACE_OUTER_BOUND('',#1106,.T.);
#679=FACE_OUTER_BOUND('',#1107,.T.);
#680=FACE_OUTER_BOUND('',#1108,.T.);
#681=FACE_OUTER_BOUND('',#1109,.T.);
#682=FACE_OUTER_BOUND('',#1110,.T.);
#683=FACE_OUTER_BOUND('',#1113,.T.);
#684=FACE_OUTER_BOUND('',#1114,.T.);
#685=FACE_OUTER_BOUND('',#1115,.T.);
#686=FACE_OUTER_BOUND('',#1116,.T.);
#687=FACE_OUTER_BOUND('',#1117,.T.);
#688=FACE_OUTER_BOUND('',#1118,.T.);
#689=FACE_OUTER_BOUND('',#1119,.T.);
#690=FACE_OUTER_BOUND('',#1120,.T.);
#691=FACE_OUTER_BOUND('',#1121,.T.);
#692=FACE_OUTER_BOUND('',#1122,.T.);
#693=FACE_OUTER_BOUND('',#1123,.T.);
#694=FACE_OUTER_BOUND('',#1124,.T.);
#695=FACE_OUTER_BOUND('',#1125,.T.);
#696=FACE_OUTER_BOUND('',#1126,.T.);
#697=FACE_OUTER_BOUND('',#1127,.T.);
#698=FACE_OUTER_BOUND('',#1128,.T.);
#699=FACE_OUTER_BOUND('',#1129,.T.);
#700=FACE_OUTER_BOUND('',#1130,.T.);
#701=FACE_OUTER_BOUND('',#1131,.T.);
#702=FACE_OUTER_BOUND('',#1132,.T.);
#703=FACE_OUTER_BOUND('',#1133,.T.);
#704=FACE_OUTER_BOUND('',#1134,.T.);
#705=FACE_OUTER_BOUND('',#1135,.T.);
#706=FACE_OUTER_BOUND('',#1136,.T.);
#707=FACE_OUTER_BOUND('',#1137,.T.);
#708=FACE_OUTER_BOUND('',#1138,.T.);
#709=FACE_OUTER_BOUND('',#1139,.T.);
#710=FACE_OUTER_BOUND('',#1140,.T.);
#711=FACE_OUTER_BOUND('',#1141,.T.);
#712=FACE_OUTER_BOUND('',#1142,.T.);
#713=FACE_OUTER_BOUND('',#1143,.T.);
#714=FACE_OUTER_BOUND('',#1144,.T.);
#715=FACE_OUTER_BOUND('',#1145,.T.);
#716=FACE_OUTER_BOUND('',#1146,.T.);
#717=FACE_OUTER_BOUND('',#1147,.T.);
#718=FACE_OUTER_BOUND('',#1148,.T.);
#719=FACE_OUTER_BOUND('',#1149,.T.);
#720=FACE_OUTER_BOUND('',#1150,.T.);
#721=FACE_OUTER_BOUND('',#1151,.T.);
#722=FACE_OUTER_BOUND('',#1152,.T.);
#723=FACE_OUTER_BOUND('',#1153,.T.);
#724=FACE_OUTER_BOUND('',#1154,.T.);
#725=FACE_OUTER_BOUND('',#1155,.T.);
#726=FACE_OUTER_BOUND('',#1156,.T.);
#727=FACE_OUTER_BOUND('',#1157,.T.);
#728=FACE_OUTER_BOUND('',#1158,.T.);
#729=FACE_OUTER_BOUND('',#1159,.T.);
#730=FACE_OUTER_BOUND('',#1160,.T.);
#731=FACE_OUTER_BOUND('',#1161,.T.);
#732=FACE_OUTER_BOUND('',#1162,.T.);
#733=FACE_OUTER_BOUND('',#1163,.T.);
#734=FACE_OUTER_BOUND('',#1164,.T.);
#735=FACE_OUTER_BOUND('',#1165,.T.);
#736=FACE_OUTER_BOUND('',#1166,.T.);
#737=FACE_OUTER_BOUND('',#1167,.T.);
#738=FACE_OUTER_BOUND('',#1168,.T.);
#739=FACE_OUTER_BOUND('',#1169,.T.);
#740=FACE_OUTER_BOUND('',#1170,.T.);
#741=FACE_OUTER_BOUND('',#1171,.T.);
#742=FACE_OUTER_BOUND('',#1172,.T.);
#743=FACE_OUTER_BOUND('',#1173,.T.);
#744=FACE_OUTER_BOUND('',#1174,.T.);
#745=FACE_OUTER_BOUND('',#1175,.T.);
#746=FACE_OUTER_BOUND('',#1176,.T.);
#747=FACE_OUTER_BOUND('',#1177,.T.);
#748=FACE_OUTER_BOUND('',#1178,.T.);
#749=FACE_OUTER_BOUND('',#1179,.T.);
#750=FACE_OUTER_BOUND('',#1180,.T.);
#751=FACE_OUTER_BOUND('',#1181,.T.);
#752=FACE_OUTER_BOUND('',#1182,.T.);
#753=FACE_OUTER_BOUND('',#1183,.T.);
#754=FACE_OUTER_BOUND('',#1184,.T.);
#755=FACE_OUTER_BOUND('',#1185,.T.);
#756=FACE_OUTER_BOUND('',#1186,.T.);
#757=FACE_OUTER_BOUND('',#1187,.T.);
#758=FACE_OUTER_BOUND('',#1188,.T.);
#759=FACE_OUTER_BOUND('',#1193,.T.);
#760=FACE_OUTER_BOUND('',#1194,.T.);
#761=FACE_OUTER_BOUND('',#1195,.T.);
#762=FACE_OUTER_BOUND('',#1196,.T.);
#763=FACE_OUTER_BOUND('',#1197,.T.);
#764=FACE_OUTER_BOUND('',#1198,.T.);
#765=FACE_OUTER_BOUND('',#1199,.T.);
#766=FACE_OUTER_BOUND('',#1200,.T.);
#767=FACE_OUTER_BOUND('',#1201,.T.);
#768=FACE_OUTER_BOUND('',#1202,.T.);
#769=FACE_OUTER_BOUND('',#1203,.T.);
#770=EDGE_LOOP('',(#3552,#3553,#3554,#3555));
#771=EDGE_LOOP('',(#3556,#3557,#3558,#3559));
#772=EDGE_LOOP('',(#3560,#3561,#3562,#3563));
#773=EDGE_LOOP('',(#3564));
#774=EDGE_LOOP('',(#3565,#3566,#3567,#3568));
#775=EDGE_LOOP('',(#3569,#3570,#3571,#3572));
#776=EDGE_LOOP('',(#3573));
#777=EDGE_LOOP('',(#3574,#3575,#3576,#3577));
#778=EDGE_LOOP('',(#3578,#3579,#3580,#3581,#3582));
#779=EDGE_LOOP('',(#3583,#3584,#3585,#3586,#3587,#3588,#3589,#3590,#3591,
#3592,#3593,#3594,#3595,#3596,#3597,#3598,#3599,#3600,#3601,#3602,#3603,
#3604,#3605,#3606));
#780=EDGE_LOOP('',(#3607));
#781=EDGE_LOOP('',(#3608));
#782=EDGE_LOOP('',(#3609,#3610,#3611,#3612,#3613,#3614));
#783=EDGE_LOOP('',(#3615,#3616,#3617,#3618,#3619));
#784=EDGE_LOOP('',(#3620,#3621,#3622,#3623,#3624,#3625));
#785=EDGE_LOOP('',(#3626,#3627,#3628,#3629,#3630));
#786=EDGE_LOOP('',(#3631,#3632,#3633,#3634,#3635,#3636,#3637,#3638,#3639,
#3640,#3641,#3642,#3643,#3644,#3645,#3646,#3647,#3648,#3649,#3650,#3651,
#3652,#3653,#3654));
#787=EDGE_LOOP('',(#3655));
#788=EDGE_LOOP('',(#3656));
#789=EDGE_LOOP('',(#3657,#3658,#3659,#3660,#3661));
#790=EDGE_LOOP('',(#3662,#3663,#3664,#3665));
#791=EDGE_LOOP('',(#3666,#3667,#3668,#3669));
#792=EDGE_LOOP('',(#3670));
#793=EDGE_LOOP('',(#3671));
#794=EDGE_LOOP('',(#3672));
#795=EDGE_LOOP('',(#3673));
#796=EDGE_LOOP('',(#3674));
#797=EDGE_LOOP('',(#3675));
#798=EDGE_LOOP('',(#3676));
#799=EDGE_LOOP('',(#3677));
#800=EDGE_LOOP('',(#3678));
#801=EDGE_LOOP('',(#3679));
#802=EDGE_LOOP('',(#3680));
#803=EDGE_LOOP('',(#3681));
#804=EDGE_LOOP('',(#3682));
#805=EDGE_LOOP('',(#3683));
#806=EDGE_LOOP('',(#3684));
#807=EDGE_LOOP('',(#3685));
#808=EDGE_LOOP('',(#3686,#3687,#3688,#3689));
#809=EDGE_LOOP('',(#3690,#3691,#3692,#3693));
#810=EDGE_LOOP('',(#3694,#3695,#3696,#3697));
#811=EDGE_LOOP('',(#3698,#3699,#3700,#3701));
#812=EDGE_LOOP('',(#3702,#3703,#3704,#3705));
#813=EDGE_LOOP('',(#3706,#3707,#3708,#3709));
#814=EDGE_LOOP('',(#3710,#3711,#3712,#3713));
#815=EDGE_LOOP('',(#3714,#3715,#3716,#3717));
#816=EDGE_LOOP('',(#3718,#3719,#3720,#3721));
#817=EDGE_LOOP('',(#3722,#3723,#3724,#3725));
#818=EDGE_LOOP('',(#3726,#3727,#3728,#3729));
#819=EDGE_LOOP('',(#3730,#3731,#3732,#3733));
#820=EDGE_LOOP('',(#3734,#3735,#3736,#3737));
#821=EDGE_LOOP('',(#3738,#3739,#3740,#3741,#3742));
#822=EDGE_LOOP('',(#3743,#3744,#3745,#3746,#3747));
#823=EDGE_LOOP('',(#3748,#3749,#3750,#3751));
#824=EDGE_LOOP('',(#3752,#3753,#3754,#3755));
#825=EDGE_LOOP('',(#3756,#3757,#3758,#3759,#3760));
#826=EDGE_LOOP('',(#3761,#3762,#3763,#3764,#3765));
#827=EDGE_LOOP('',(#3766,#3767,#3768,#3769));
#828=EDGE_LOOP('',(#3770,#3771,#3772,#3773));
#829=EDGE_LOOP('',(#3774,#3775,#3776,#3777));
#830=EDGE_LOOP('',(#3778,#3779,#3780,#3781));
#831=EDGE_LOOP('',(#3782,#3783,#3784,#3785));
#832=EDGE_LOOP('',(#3786,#3787,#3788,#3789));
#833=EDGE_LOOP('',(#3790,#3791,#3792,#3793));
#834=EDGE_LOOP('',(#3794,#3795,#3796,#3797));
#835=EDGE_LOOP('',(#3798,#3799,#3800,#3801));
#836=EDGE_LOOP('',(#3802,#3803,#3804,#3805));
#837=EDGE_LOOP('',(#3806,#3807,#3808,#3809));
#838=EDGE_LOOP('',(#3810,#3811,#3812,#3813));
#839=EDGE_LOOP('',(#3814,#3815,#3816,#3817));
#840=EDGE_LOOP('',(#3818,#3819,#3820,#3821));
#841=EDGE_LOOP('',(#3822,#3823,#3824,#3825));
#842=EDGE_LOOP('',(#3826,#3827,#3828,#3829));
#843=EDGE_LOOP('',(#3830,#3831,#3832,#3833));
#844=EDGE_LOOP('',(#3834,#3835,#3836,#3837));
#845=EDGE_LOOP('',(#3838,#3839,#3840,#3841));
#846=EDGE_LOOP('',(#3842,#3843,#3844,#3845));
#847=EDGE_LOOP('',(#3846,#3847,#3848));
#848=EDGE_LOOP('',(#3849,#3850,#3851));
#849=EDGE_LOOP('',(#3852,#3853,#3854,#3855));
#850=EDGE_LOOP('',(#3856,#3857,#3858,#3859));
#851=EDGE_LOOP('',(#3860,#3861,#3862));
#852=EDGE_LOOP('',(#3863,#3864,#3865,#3866));
#853=EDGE_LOOP('',(#3867,#3868,#3869,#3870));
#854=EDGE_LOOP('',(#3871,#3872,#3873));
#855=EDGE_LOOP('',(#3874,#3875,#3876,#3877));
#856=EDGE_LOOP('',(#3878,#3879,#3880,#3881));
#857=EDGE_LOOP('',(#3882,#3883,#3884,#3885));
#858=EDGE_LOOP('',(#3886,#3887,#3888,#3889));
#859=EDGE_LOOP('',(#3890,#3891,#3892,#3893));
#860=EDGE_LOOP('',(#3894,#3895,#3896));
#861=EDGE_LOOP('',(#3897,#3898,#3899,#3900));
#862=EDGE_LOOP('',(#3901,#3902,#3903));
#863=EDGE_LOOP('',(#3904,#3905,#3906,#3907));
#864=EDGE_LOOP('',(#3908,#3909,#3910,#3911));
#865=EDGE_LOOP('',(#3912,#3913,#3914));
#866=EDGE_LOOP('',(#3915,#3916,#3917,#3918));
#867=EDGE_LOOP('',(#3919,#3920,#3921));
#868=EDGE_LOOP('',(#3922,#3923,#3924,#3925));
#869=EDGE_LOOP('',(#3926,#3927,#3928,#3929));
#870=EDGE_LOOP('',(#3930,#3931,#3932,#3933));
#871=EDGE_LOOP('',(#3934,#3935,#3936,#3937));
#872=EDGE_LOOP('',(#3938,#3939,#3940,#3941));
#873=EDGE_LOOP('',(#3942,#3943,#3944));
#874=EDGE_LOOP('',(#3945,#3946,#3947,#3948));
#875=EDGE_LOOP('',(#3949,#3950,#3951));
#876=EDGE_LOOP('',(#3952,#3953,#3954,#3955));
#877=EDGE_LOOP('',(#3956,#3957,#3958,#3959));
#878=EDGE_LOOP('',(#3960,#3961,#3962));
#879=EDGE_LOOP('',(#3963,#3964,#3965));
#880=EDGE_LOOP('',(#3966,#3967,#3968));
#881=EDGE_LOOP('',(#3969,#3970,#3971,#3972));
#882=EDGE_LOOP('',(#3973,#3974,#3975));
#883=EDGE_LOOP('',(#3976,#3977,#3978,#3979));
#884=EDGE_LOOP('',(#3980,#3981,#3982,#3983));
#885=EDGE_LOOP('',(#3984,#3985,#3986));
#886=EDGE_LOOP('',(#3987,#3988,#3989));
#887=EDGE_LOOP('',(#3990,#3991,#3992,#3993));
#888=EDGE_LOOP('',(#3994,#3995,#3996,#3997));
#889=EDGE_LOOP('',(#3998,#3999,#4000,#4001));
#890=EDGE_LOOP('',(#4002,#4003,#4004,#4005));
#891=EDGE_LOOP('',(#4006,#4007,#4008,#4009));
#892=EDGE_LOOP('',(#4010,#4011,#4012,#4013));
#893=EDGE_LOOP('',(#4014,#4015,#4016,#4017));
#894=EDGE_LOOP('',(#4018,#4019,#4020,#4021));
#895=EDGE_LOOP('',(#4022,#4023,#4024,#4025));
#896=EDGE_LOOP('',(#4026,#4027,#4028,#4029));
#897=EDGE_LOOP('',(#4030,#4031,#4032,#4033));
#898=EDGE_LOOP('',(#4034,#4035,#4036,#4037));
#899=EDGE_LOOP('',(#4038,#4039,#4040,#4041));
#900=EDGE_LOOP('',(#4042,#4043,#4044,#4045));
#901=EDGE_LOOP('',(#4046,#4047,#4048,#4049));
#902=EDGE_LOOP('',(#4050,#4051,#4052,#4053));
#903=EDGE_LOOP('',(#4054,#4055,#4056,#4057));
#904=EDGE_LOOP('',(#4058,#4059,#4060,#4061));
#905=EDGE_LOOP('',(#4062,#4063,#4064,#4065));
#906=EDGE_LOOP('',(#4066,#4067,#4068,#4069));
#907=EDGE_LOOP('',(#4070,#4071,#4072,#4073));
#908=EDGE_LOOP('',(#4074,#4075,#4076,#4077));
#909=EDGE_LOOP('',(#4078,#4079,#4080,#4081));
#910=EDGE_LOOP('',(#4082,#4083,#4084,#4085));
#911=EDGE_LOOP('',(#4086,#4087,#4088,#4089));
#912=EDGE_LOOP('',(#4090,#4091,#4092,#4093));
#913=EDGE_LOOP('',(#4094,#4095,#4096,#4097));
#914=EDGE_LOOP('',(#4098,#4099,#4100,#4101));
#915=EDGE_LOOP('',(#4102,#4103,#4104,#4105));
#916=EDGE_LOOP('',(#4106,#4107,#4108,#4109));
#917=EDGE_LOOP('',(#4110,#4111,#4112,#4113));
#918=EDGE_LOOP('',(#4114,#4115,#4116,#4117));
#919=EDGE_LOOP('',(#4118,#4119,#4120,#4121));
#920=EDGE_LOOP('',(#4122,#4123,#4124,#4125));
#921=EDGE_LOOP('',(#4126,#4127,#4128,#4129));
#922=EDGE_LOOP('',(#4130,#4131,#4132,#4133));
#923=EDGE_LOOP('',(#4134,#4135,#4136,#4137));
#924=EDGE_LOOP('',(#4138,#4139,#4140,#4141));
#925=EDGE_LOOP('',(#4142,#4143,#4144,#4145));
#926=EDGE_LOOP('',(#4146,#4147,#4148,#4149));
#927=EDGE_LOOP('',(#4150,#4151,#4152,#4153));
#928=EDGE_LOOP('',(#4154,#4155,#4156,#4157));
#929=EDGE_LOOP('',(#4158,#4159,#4160,#4161));
#930=EDGE_LOOP('',(#4162,#4163,#4164,#4165));
#931=EDGE_LOOP('',(#4166,#4167,#4168,#4169));
#932=EDGE_LOOP('',(#4170,#4171,#4172,#4173));
#933=EDGE_LOOP('',(#4174,#4175,#4176,#4177));
#934=EDGE_LOOP('',(#4178,#4179,#4180,#4181));
#935=EDGE_LOOP('',(#4182));
#936=EDGE_LOOP('',(#4183));
#937=EDGE_LOOP('',(#4184));
#938=EDGE_LOOP('',(#4185));
#939=EDGE_LOOP('',(#4186));
#940=EDGE_LOOP('',(#4187));
#941=EDGE_LOOP('',(#4188));
#942=EDGE_LOOP('',(#4189));
#943=EDGE_LOOP('',(#4190));
#944=EDGE_LOOP('',(#4191));
#945=EDGE_LOOP('',(#4192));
#946=EDGE_LOOP('',(#4193));
#947=EDGE_LOOP('',(#4194));
#948=EDGE_LOOP('',(#4195));
#949=EDGE_LOOP('',(#4196));
#950=EDGE_LOOP('',(#4197));
#951=EDGE_LOOP('',(#4198,#4199,#4200,#4201,#4202));
#952=EDGE_LOOP('',(#4203));
#953=EDGE_LOOP('',(#4204));
#954=EDGE_LOOP('',(#4205,#4206,#4207,#4208,#4209,#4210));
#955=EDGE_LOOP('',(#4211,#4212,#4213,#4214,#4215));
#956=EDGE_LOOP('',(#4216,#4217,#4218,#4219,#4220,#4221));
#957=EDGE_LOOP('',(#4222,#4223,#4224,#4225,#4226));
#958=EDGE_LOOP('',(#4227));
#959=EDGE_LOOP('',(#4228));
#960=EDGE_LOOP('',(#4229,#4230,#4231,#4232,#4233));
#961=EDGE_LOOP('',(#4234,#4235,#4236,#4237,#4238));
#962=EDGE_LOOP('',(#4239));
#963=EDGE_LOOP('',(#4240));
#964=EDGE_LOOP('',(#4241,#4242,#4243,#4244,#4245,#4246));
#965=EDGE_LOOP('',(#4247,#4248,#4249,#4250,#4251));
#966=EDGE_LOOP('',(#4252,#4253,#4254,#4255,#4256,#4257));
#967=EDGE_LOOP('',(#4258,#4259,#4260,#4261,#4262));
#968=EDGE_LOOP('',(#4263));
#969=EDGE_LOOP('',(#4264));
#970=EDGE_LOOP('',(#4265,#4266,#4267,#4268,#4269));
#971=EDGE_LOOP('',(#4270,#4271,#4272,#4273));
#972=EDGE_LOOP('',(#4274,#4275,#4276,#4277));
#973=EDGE_LOOP('',(#4278));
#974=EDGE_LOOP('',(#4279));
#975=EDGE_LOOP('',(#4280,#4281,#4282,#4283));
#976=EDGE_LOOP('',(#4284,#4285,#4286,#4287));
#977=EDGE_LOOP('',(#4288,#4289,#4290,#4291));
#978=EDGE_LOOP('',(#4292,#4293,#4294,#4295,#4296));
#979=EDGE_LOOP('',(#4297,#4298,#4299,#4300));
#980=EDGE_LOOP('',(#4301));
#981=EDGE_LOOP('',(#4302));
#982=EDGE_LOOP('',(#4303,#4304,#4305,#4306,#4307));
#983=EDGE_LOOP('',(#4308,#4309,#4310,#4311,#4312));
#984=EDGE_LOOP('',(#4313,#4314,#4315,#4316,#4317));
#985=EDGE_LOOP('',(#4318,#4319,#4320));
#986=EDGE_LOOP('',(#4321,#4322,#4323));
#987=EDGE_LOOP('',(#4324,#4325,#4326));
#988=EDGE_LOOP('',(#4327,#4328,#4329,#4330));
#989=EDGE_LOOP('',(#4331,#4332,#4333));
#990=EDGE_LOOP('',(#4334,#4335,#4336,#4337));
#991=EDGE_LOOP('',(#4338,#4339,#4340));
#992=EDGE_LOOP('',(#4341,#4342,#4343,#4344));
#993=EDGE_LOOP('',(#4345,#4346,#4347,#4348));
#994=EDGE_LOOP('',(#4349,#4350,#4351));
#995=EDGE_LOOP('',(#4352,#4353,#4354,#4355));
#996=EDGE_LOOP('',(#4356,#4357,#4358));
#997=EDGE_LOOP('',(#4359,#4360,#4361,#4362));
#998=EDGE_LOOP('',(#4363,#4364,#4365));
#999=EDGE_LOOP('',(#4366,#4367,#4368,#4369));
#1000=EDGE_LOOP('',(#4370,#4371,#4372,#4373));
#1001=EDGE_LOOP('',(#4374,#4375,#4376,#4377));
#1002=EDGE_LOOP('',(#4378,#4379,#4380));
#1003=EDGE_LOOP('',(#4381,#4382,#4383,#4384));
#1004=EDGE_LOOP('',(#4385,#4386,#4387,#4388));
#1005=EDGE_LOOP('',(#4389,#4390,#4391));
#1006=EDGE_LOOP('',(#4392,#4393,#4394,#4395));
#1007=EDGE_LOOP('',(#4396,#4397,#4398));
#1008=EDGE_LOOP('',(#4399,#4400,#4401,#4402));
#1009=EDGE_LOOP('',(#4403,#4404,#4405));
#1010=EDGE_LOOP('',(#4406,#4407,#4408,#4409));
#1011=EDGE_LOOP('',(#4410,#4411,#4412));
#1012=EDGE_LOOP('',(#4413,#4414,#4415,#4416));
#1013=EDGE_LOOP('',(#4417,#4418,#4419,#4420));
#1014=EDGE_LOOP('',(#4421,#4422,#4423));
#1015=EDGE_LOOP('',(#4424,#4425,#4426));
#1016=EDGE_LOOP('',(#4427,#4428,#4429,#4430));
#1017=EDGE_LOOP('',(#4431,#4432,#4433));
#1018=EDGE_LOOP('',(#4434,#4435,#4436,#4437));
#1019=EDGE_LOOP('',(#4438,#4439,#4440,#4441));
#1020=EDGE_LOOP('',(#4442,#4443,#4444,#4445));
#1021=EDGE_LOOP('',(#4446,#4447,#4448,#4449));
#1022=EDGE_LOOP('',(#4450,#4451,#4452,#4453));
#1023=EDGE_LOOP('',(#4454,#4455,#4456));
#1024=EDGE_LOOP('',(#4457,#4458,#4459));
#1025=EDGE_LOOP('',(#4460,#4461,#4462));
#1026=EDGE_LOOP('',(#4463,#4464,#4465,#4466));
#1027=EDGE_LOOP('',(#4467,#4468,#4469));
#1028=EDGE_LOOP('',(#4470,#4471,#4472,#4473));
#1029=EDGE_LOOP('',(#4474,#4475,#4476,#4477));
#1030=EDGE_LOOP('',(#4478,#4479,#4480,#4481));
#1031=EDGE_LOOP('',(#4482,#4483,#4484,#4485));
#1032=EDGE_LOOP('',(#4486,#4487,#4488,#4489));
#1033=EDGE_LOOP('',(#4490,#4491,#4492,#4493));
#1034=EDGE_LOOP('',(#4494,#4495,#4496,#4497));
#1035=EDGE_LOOP('',(#4498,#4499,#4500,#4501));
#1036=EDGE_LOOP('',(#4502,#4503,#4504,#4505));
#1037=EDGE_LOOP('',(#4506,#4507,#4508,#4509));
#1038=EDGE_LOOP('',(#4510,#4511,#4512,#4513));
#1039=EDGE_LOOP('',(#4514,#4515,#4516,#4517));
#1040=EDGE_LOOP('',(#4518,#4519,#4520,#4521));
#1041=EDGE_LOOP('',(#4522,#4523,#4524,#4525));
#1042=EDGE_LOOP('',(#4526,#4527,#4528,#4529));
#1043=EDGE_LOOP('',(#4530,#4531,#4532,#4533));
#1044=EDGE_LOOP('',(#4534,#4535,#4536,#4537));
#1045=EDGE_LOOP('',(#4538,#4539,#4540,#4541));
#1046=EDGE_LOOP('',(#4542,#4543,#4544,#4545));
#1047=EDGE_LOOP('',(#4546,#4547,#4548,#4549));
#1048=EDGE_LOOP('',(#4550,#4551,#4552,#4553));
#1049=EDGE_LOOP('',(#4554,#4555,#4556,#4557));
#1050=EDGE_LOOP('',(#4558,#4559,#4560,#4561));
#1051=EDGE_LOOP('',(#4562,#4563,#4564,#4565));
#1052=EDGE_LOOP('',(#4566,#4567,#4568,#4569));
#1053=EDGE_LOOP('',(#4570,#4571,#4572,#4573));
#1054=EDGE_LOOP('',(#4574,#4575,#4576,#4577));
#1055=EDGE_LOOP('',(#4578,#4579,#4580,#4581));
#1056=EDGE_LOOP('',(#4582,#4583,#4584,#4585));
#1057=EDGE_LOOP('',(#4586,#4587,#4588,#4589));
#1058=EDGE_LOOP('',(#4590));
#1059=EDGE_LOOP('',(#4591));
#1060=EDGE_LOOP('',(#4592));
#1061=EDGE_LOOP('',(#4593));
#1062=EDGE_LOOP('',(#4594,#4595,#4596,#4597));
#1063=EDGE_LOOP('',(#4598,#4599,#4600,#4601));
#1064=EDGE_LOOP('',(#4602,#4603,#4604,#4605));
#1065=EDGE_LOOP('',(#4606,#4607,#4608,#4609));
#1066=EDGE_LOOP('',(#4610,#4611,#4612,#4613));
#1067=EDGE_LOOP('',(#4614,#4615,#4616,#4617));
#1068=EDGE_LOOP('',(#4618,#4619,#4620,#4621,#4622,#4623,#4624,#4625,#4626,
#4627,#4628,#4629,#4630,#4631,#4632,#4633,#4634,#4635));
#1069=EDGE_LOOP('',(#4636,#4637,#4638,#4639));
#1070=EDGE_LOOP('',(#4640,#4641,#4642,#4643,#4644,#4645,#4646,#4647,#4648,
#4649,#4650,#4651,#4652,#4653,#4654,#4655,#4656,#4657));
#1071=EDGE_LOOP('',(#4658,#4659,#4660,#4661));
#1072=EDGE_LOOP('',(#4662,#4663,#4664,#4665));
#1073=EDGE_LOOP('',(#4666));
#1074=EDGE_LOOP('',(#4667,#4668,#4669,#4670));
#1075=EDGE_LOOP('',(#4671));
#1076=EDGE_LOOP('',(#4672,#4673,#4674,#4675,#4676));
#1077=EDGE_LOOP('',(#4677));
#1078=EDGE_LOOP('',(#4678));
#1079=EDGE_LOOP('',(#4679,#4680,#4681,#4682,#4683,#4684));
#1080=EDGE_LOOP('',(#4685,#4686,#4687,#4688,#4689));
#1081=EDGE_LOOP('',(#4690,#4691,#4692,#4693,#4694,#4695));
#1082=EDGE_LOOP('',(#4696,#4697,#4698,#4699,#4700));
#1083=EDGE_LOOP('',(#4701));
#1084=EDGE_LOOP('',(#4702));
#1085=EDGE_LOOP('',(#4703,#4704,#4705,#4706,#4707));
#1086=EDGE_LOOP('',(#4708));
#1087=EDGE_LOOP('',(#4709,#4710,#4711,#4712));
#1088=EDGE_LOOP('',(#4713));
#1089=EDGE_LOOP('',(#4714));
#1090=EDGE_LOOP('',(#4715,#4716,#4717,#4718));
#1091=EDGE_LOOP('',(#4719));
#1092=EDGE_LOOP('',(#4720,#4721,#4722,#4723,#4724));
#1093=EDGE_LOOP('',(#4725));
#1094=EDGE_LOOP('',(#4726));
#1095=EDGE_LOOP('',(#4727,#4728,#4729,#4730,#4731,#4732));
#1096=EDGE_LOOP('',(#4733,#4734,#4735,#4736,#4737));
#1097=EDGE_LOOP('',(#4738,#4739,#4740,#4741,#4742,#4743));
#1098=EDGE_LOOP('',(#4744,#4745,#4746,#4747,#4748));
#1099=EDGE_LOOP('',(#4749));
#1100=EDGE_LOOP('',(#4750));
#1101=EDGE_LOOP('',(#4751,#4752,#4753,#4754,#4755));
#1102=EDGE_LOOP('',(#4756,#4757,#4758,#4759));
#1103=EDGE_LOOP('',(#4760,#4761,#4762,#4763));
#1104=EDGE_LOOP('',(#4764));
#1105=EDGE_LOOP('',(#4765));
#1106=EDGE_LOOP('',(#4766,#4767,#4768,#4769));
#1107=EDGE_LOOP('',(#4770,#4771,#4772,#4773));
#1108=EDGE_LOOP('',(#4774,#4775,#4776,#4777));
#1109=EDGE_LOOP('',(#4778,#4779,#4780,#4781,#4782));
#1110=EDGE_LOOP('',(#4783,#4784,#4785,#4786));
#1111=EDGE_LOOP('',(#4787));
#1112=EDGE_LOOP('',(#4788));
#1113=EDGE_LOOP('',(#4789,#4790,#4791,#4792,#4793));
#1114=EDGE_LOOP('',(#4794,#4795,#4796,#4797,#4798));
#1115=EDGE_LOOP('',(#4799,#4800,#4801,#4802,#4803));
#1116=EDGE_LOOP('',(#4804,#4805,#4806));
#1117=EDGE_LOOP('',(#4807,#4808,#4809));
#1118=EDGE_LOOP('',(#4810,#4811,#4812));
#1119=EDGE_LOOP('',(#4813,#4814,#4815,#4816));
#1120=EDGE_LOOP('',(#4817,#4818,#4819));
#1121=EDGE_LOOP('',(#4820,#4821,#4822,#4823));
#1122=EDGE_LOOP('',(#4824,#4825,#4826));
#1123=EDGE_LOOP('',(#4827,#4828,#4829,#4830));
#1124=EDGE_LOOP('',(#4831,#4832,#4833,#4834));
#1125=EDGE_LOOP('',(#4835,#4836,#4837));
#1126=EDGE_LOOP('',(#4838,#4839,#4840,#4841));
#1127=EDGE_LOOP('',(#4842,#4843,#4844));
#1128=EDGE_LOOP('',(#4845,#4846,#4847,#4848));
#1129=EDGE_LOOP('',(#4849,#4850,#4851));
#1130=EDGE_LOOP('',(#4852,#4853,#4854,#4855));
#1131=EDGE_LOOP('',(#4856,#4857,#4858,#4859));
#1132=EDGE_LOOP('',(#4860,#4861,#4862,#4863));
#1133=EDGE_LOOP('',(#4864,#4865,#4866));
#1134=EDGE_LOOP('',(#4867,#4868,#4869,#4870));
#1135=EDGE_LOOP('',(#4871,#4872,#4873,#4874));
#1136=EDGE_LOOP('',(#4875,#4876,#4877));
#1137=EDGE_LOOP('',(#4878,#4879,#4880,#4881));
#1138=EDGE_LOOP('',(#4882,#4883,#4884));
#1139=EDGE_LOOP('',(#4885,#4886,#4887,#4888));
#1140=EDGE_LOOP('',(#4889,#4890,#4891));
#1141=EDGE_LOOP('',(#4892,#4893,#4894,#4895));
#1142=EDGE_LOOP('',(#4896,#4897,#4898));
#1143=EDGE_LOOP('',(#4899,#4900,#4901,#4902));
#1144=EDGE_LOOP('',(#4903,#4904,#4905,#4906));
#1145=EDGE_LOOP('',(#4907,#4908,#4909));
#1146=EDGE_LOOP('',(#4910,#4911,#4912));
#1147=EDGE_LOOP('',(#4913,#4914,#4915,#4916));
#1148=EDGE_LOOP('',(#4917,#4918,#4919));
#1149=EDGE_LOOP('',(#4920,#4921,#4922,#4923));
#1150=EDGE_LOOP('',(#4924,#4925,#4926,#4927));
#1151=EDGE_LOOP('',(#4928,#4929,#4930,#4931));
#1152=EDGE_LOOP('',(#4932,#4933,#4934,#4935));
#1153=EDGE_LOOP('',(#4936,#4937,#4938,#4939));
#1154=EDGE_LOOP('',(#4940,#4941,#4942));
#1155=EDGE_LOOP('',(#4943,#4944,#4945));
#1156=EDGE_LOOP('',(#4946,#4947,#4948));
#1157=EDGE_LOOP('',(#4949,#4950,#4951,#4952));
#1158=EDGE_LOOP('',(#4953,#4954,#4955));
#1159=EDGE_LOOP('',(#4956,#4957,#4958,#4959));
#1160=EDGE_LOOP('',(#4960,#4961,#4962,#4963));
#1161=EDGE_LOOP('',(#4964,#4965,#4966,#4967));
#1162=EDGE_LOOP('',(#4968,#4969,#4970,#4971));
#1163=EDGE_LOOP('',(#4972,#4973,#4974,#4975));
#1164=EDGE_LOOP('',(#4976,#4977,#4978,#4979));
#1165=EDGE_LOOP('',(#4980,#4981,#4982,#4983));
#1166=EDGE_LOOP('',(#4984,#4985,#4986,#4987));
#1167=EDGE_LOOP('',(#4988,#4989,#4990,#4991));
#1168=EDGE_LOOP('',(#4992,#4993,#4994,#4995));
#1169=EDGE_LOOP('',(#4996,#4997,#4998,#4999));
#1170=EDGE_LOOP('',(#5000,#5001,#5002,#5003));
#1171=EDGE_LOOP('',(#5004,#5005,#5006,#5007));
#1172=EDGE_LOOP('',(#5008,#5009,#5010,#5011));
#1173=EDGE_LOOP('',(#5012,#5013,#5014,#5015));
#1174=EDGE_LOOP('',(#5016,#5017,#5018,#5019));
#1175=EDGE_LOOP('',(#5020,#5021,#5022,#5023));
#1176=EDGE_LOOP('',(#5024,#5025,#5026,#5027));
#1177=EDGE_LOOP('',(#5028,#5029,#5030,#5031));
#1178=EDGE_LOOP('',(#5032,#5033,#5034,#5035));
#1179=EDGE_LOOP('',(#5036,#5037,#5038,#5039));
#1180=EDGE_LOOP('',(#5040,#5041,#5042,#5043));
#1181=EDGE_LOOP('',(#5044,#5045,#5046,#5047));
#1182=EDGE_LOOP('',(#5048,#5049,#5050,#5051));
#1183=EDGE_LOOP('',(#5052,#5053,#5054,#5055));
#1184=EDGE_LOOP('',(#5056,#5057,#5058,#5059));
#1185=EDGE_LOOP('',(#5060,#5061,#5062,#5063));
#1186=EDGE_LOOP('',(#5064,#5065,#5066,#5067));
#1187=EDGE_LOOP('',(#5068,#5069,#5070,#5071));
#1188=EDGE_LOOP('',(#5072,#5073,#5074,#5075));
#1189=EDGE_LOOP('',(#5076));
#1190=EDGE_LOOP('',(#5077));
#1191=EDGE_LOOP('',(#5078));
#1192=EDGE_LOOP('',(#5079));
#1193=EDGE_LOOP('',(#5080,#5081,#5082,#5083));
#1194=EDGE_LOOP('',(#5084,#5085,#5086,#5087));
#1195=EDGE_LOOP('',(#5088,#5089,#5090,#5091));
#1196=EDGE_LOOP('',(#5092,#5093,#5094,#5095));
#1197=EDGE_LOOP('',(#5096,#5097,#5098,#5099));
#1198=EDGE_LOOP('',(#5100,#5101,#5102,#5103));
#1199=EDGE_LOOP('',(#5104,#5105,#5106,#5107,#5108,#5109,#5110,#5111,#5112,
#5113,#5114,#5115,#5116,#5117,#5118,#5119,#5120,#5121));
#1200=EDGE_LOOP('',(#5122,#5123,#5124,#5125));
#1201=EDGE_LOOP('',(#5126,#5127,#5128,#5129,#5130,#5131,#5132,#5133,#5134,
#5135,#5136,#5137,#5138,#5139,#5140,#5141,#5142,#5143));
#1202=EDGE_LOOP('',(#5144,#5145,#5146,#5147));
#1203=EDGE_LOOP('',(#5148,#5149,#5150,#5151));
#1204=LINE('',#8756,#1534);
#1205=LINE('',#8761,#1535);
#1206=LINE('',#8763,#1536);
#1207=LINE('',#8765,#1537);
#1208=LINE('',#8766,#1538);
#1209=LINE('',#8769,#1539);
#1210=LINE('',#8771,#1540);
#1211=LINE('',#8772,#1541);
#1212=LINE('',#8775,#1542);
#1213=LINE('',#8777,#1543);
#1214=LINE('',#8778,#1544);
#1215=LINE('',#8780,#1545);
#1216=LINE('',#8781,#1546);
#1217=LINE('',#8794,#1547);
#1218=LINE('',#8796,#1548);
#1219=LINE('',#8800,#1549);
#1220=LINE('',#8802,#1550);
#1221=LINE('',#8806,#1551);
#1222=LINE('',#8808,#1552);
#1223=LINE('',#8810,#1553);
#1224=LINE('',#8812,#1554);
#1225=LINE('',#8814,#1555);
#1226=LINE('',#8816,#1556);
#1227=LINE('',#8818,#1557);
#1228=LINE('',#8820,#1558);
#1229=LINE('',#8822,#1559);
#1230=LINE('',#8824,#1560);
#1231=LINE('',#8826,#1561);
#1232=LINE('',#8830,#1562);
#1233=LINE('',#8832,#1563);
#1234=LINE('',#8836,#1564);
#1235=LINE('',#8838,#1565);
#1236=LINE('',#8839,#1566);
#1237=LINE('',#8844,#1567);
#1238=LINE('',#8856,#1568);
#1239=LINE('',#8869,#1569);
#1240=LINE('',#8871,#1570);
#1241=LINE('',#8873,#1571);
#1242=LINE('',#8875,#1572);
#1243=LINE('',#8877,#1573);
#1244=LINE('',#8881,#1574);
#1245=LINE('',#8883,#1575);
#1246=LINE('',#8887,#1576);
#1247=LINE('',#8889,#1577);
#1248=LINE('',#8891,#1578);
#1249=LINE('',#8893,#1579);
#1250=LINE('',#8895,#1580);
#1251=LINE('',#8897,#1581);
#1252=LINE('',#8899,#1582);
#1253=LINE('',#8901,#1583);
#1254=LINE('',#8903,#1584);
#1255=LINE('',#8905,#1585);
#1256=LINE('',#8907,#1586);
#1257=LINE('',#8911,#1587);
#1258=LINE('',#8912,#1588);
#1259=LINE('',#8926,#1589);
#1260=LINE('',#8928,#1590);
#1261=LINE('',#8930,#1591);
#1262=LINE('',#8931,#1592);
#1263=LINE('',#8964,#1593);
#1264=LINE('',#8972,#1594);
#1265=LINE('',#8980,#1595);
#1266=LINE('',#8988,#1596);
#1267=LINE('',#8996,#1597);
#1268=LINE('',#9004,#1598);
#1269=LINE('',#9012,#1599);
#1270=LINE('',#9022,#1600);
#1271=LINE('',#9030,#1601);
#1272=LINE('',#9040,#1602);
#1273=LINE('',#9048,#1603);
#1274=LINE('',#9056,#1604);
#1275=LINE('',#9064,#1605);
#1276=LINE('',#9072,#1606);
#1277=LINE('',#9080,#1607);
#1278=LINE('',#9088,#1608);
#1279=LINE('',#9094,#1609);
#1280=LINE('',#9100,#1610);
#1281=LINE('',#9105,#1611);
#1282=LINE('',#9109,#1612);
#1283=LINE('',#9113,#1613);
#1284=LINE('',#9117,#1614);
#1285=LINE('',#9121,#1615);
#1286=LINE('',#9127,#1616);
#1287=LINE('',#9141,#1617);
#1288=LINE('',#9142,#1618);
#1289=LINE('',#9144,#1619);
#1290=LINE('',#9153,#1620);
#1291=LINE('',#9169,#1621);
#1292=LINE('',#9172,#1622);
#1293=LINE('',#9173,#1623);
#1294=LINE('',#9181,#1624);
#1295=LINE('',#9207,#1625);
#1296=LINE('',#9208,#1626);
#1297=LINE('',#9210,#1627);
#1298=LINE('',#9230,#1628);
#1299=LINE('',#9231,#1629);
#1300=LINE('',#9239,#1630);
#1301=LINE('',#9247,#1631);
#1302=LINE('',#9267,#1632);
#1303=LINE('',#9268,#1633);
#1304=LINE('',#9270,#1634);
#1305=LINE('',#9289,#1635);
#1306=LINE('',#9290,#1636);
#1307=LINE('',#9297,#1637);
#1308=LINE('',#9299,#1638);
#1309=LINE('',#9311,#1639);
#1310=LINE('',#9314,#1640);
#1311=LINE('',#9316,#1641);
#1312=LINE('',#9319,#1642);
#1313=LINE('',#9321,#1643);
#1314=LINE('',#9323,#1644);
#1315=LINE('',#9325,#1645);
#1316=LINE('',#9327,#1646);
#1317=LINE('',#9328,#1647);
#1318=LINE('',#9330,#1648);
#1319=LINE('',#9332,#1649);
#1320=LINE('',#9333,#1650);
#1321=LINE('',#9335,#1651);
#1322=LINE('',#9337,#1652);
#1323=LINE('',#9339,#1653);
#1324=LINE('',#9341,#1654);
#1325=LINE('',#9343,#1655);
#1326=LINE('',#9344,#1656);
#1327=LINE('',#9346,#1657);
#1328=LINE('',#9348,#1658);
#1329=LINE('',#9350,#1659);
#1330=LINE('',#9351,#1660);
#1331=LINE('',#9353,#1661);
#1332=LINE('',#9355,#1662);
#1333=LINE('',#9358,#1663);
#1334=LINE('',#9361,#1664);
#1335=LINE('',#9364,#1665);
#1336=LINE('',#9367,#1666);
#1337=LINE('',#9370,#1667);
#1338=LINE('',#9373,#1668);
#1339=LINE('',#9375,#1669);
#1340=LINE('',#9376,#1670);
#1341=LINE('',#9378,#1671);
#1342=LINE('',#9380,#1672);
#1343=LINE('',#9382,#1673);
#1344=LINE('',#9384,#1674);
#1345=LINE('',#9386,#1675);
#1346=LINE('',#9388,#1676);
#1347=LINE('',#9431,#1677);
#1348=LINE('',#9443,#1678);
#1349=LINE('',#9470,#1679);
#1350=LINE('',#9482,#1680);
#1351=LINE('',#9505,#1681);
#1352=LINE('',#9507,#1682);
#1353=LINE('',#9509,#1683);
#1354=LINE('',#9510,#1684);
#1355=LINE('',#9515,#1685);
#1356=LINE('',#9523,#1686);
#1357=LINE('',#9536,#1687);
#1358=LINE('',#9538,#1688);
#1359=LINE('',#9540,#1689);
#1360=LINE('',#9541,#1690);
#1361=LINE('',#9546,#1691);
#1362=LINE('',#9556,#1692);
#1363=LINE('',#9580,#1693);
#1364=LINE('',#9581,#1694);
#1365=LINE('',#9589,#1695);
#1366=LINE('',#9590,#1696);
#1367=LINE('',#9599,#1697);
#1368=LINE('',#9600,#1698);
#1369=LINE('',#9602,#1699);
#1370=LINE('',#9603,#1700);
#1371=LINE('',#9611,#1701);
#1372=LINE('',#9612,#1702);
#1373=LINE('',#9634,#1703);
#1374=LINE('',#9659,#1704);
#1375=LINE('',#9660,#1705);
#1376=LINE('',#9677,#1706);
#1377=LINE('',#9678,#1707);
#1378=LINE('',#9687,#1708);
#1379=LINE('',#9688,#1709);
#1380=LINE('',#9697,#1710);
#1381=LINE('',#9698,#1711);
#1382=LINE('',#9707,#1712);
#1383=LINE('',#9708,#1713);
#1384=LINE('',#9710,#1714);
#1385=LINE('',#9711,#1715);
#1386=LINE('',#9728,#1716);
#1387=LINE('',#9744,#1717);
#1388=LINE('',#9753,#1718);
#1389=LINE('',#9754,#1719);
#1390=LINE('',#9756,#1720);
#1391=LINE('',#9757,#1721);
#1392=LINE('',#9760,#1722);
#1393=LINE('',#9776,#1723);
#1394=LINE('',#9779,#1724);
#1395=LINE('',#9795,#1725);
#1396=LINE('',#9798,#1726);
#1397=LINE('',#9814,#1727);
#1398=LINE('',#9837,#1728);
#1399=LINE('',#9838,#1729);
#1400=LINE('',#9848,#1730);
#1401=LINE('',#9864,#1731);
#1402=LINE('',#9866,#1732);
#1403=LINE('',#9867,#1733);
#1404=LINE('',#9869,#1734);
#1405=LINE('',#9870,#1735);
#1406=LINE('',#9873,#1736);
#1407=LINE('',#9889,#1737);
#1408=LINE('',#9891,#1738);
#1409=LINE('',#9892,#1739);
#1410=LINE('',#9895,#1740);
#1411=LINE('',#9911,#1741);
#1412=LINE('',#9917,#1742);
#1413=LINE('',#9933,#1743);
#1414=LINE('',#9944,#1744);
#1415=LINE('',#9945,#1745);
#1416=LINE('',#9947,#1746);
#1417=LINE('',#9948,#1747);
#1418=LINE('',#9950,#1748);
#1419=LINE('',#9951,#1749);
#1420=LINE('',#9953,#1750);
#1421=LINE('',#9954,#1751);
#1422=LINE('',#9956,#1752);
#1423=LINE('',#9958,#1753);
#1424=LINE('',#9960,#1754);
#1425=LINE('',#9962,#1755);
#1426=LINE('',#9964,#1756);
#1427=LINE('',#9966,#1757);
#1428=LINE('',#9967,#1758);
#1429=LINE('',#9969,#1759);
#1430=LINE('',#9971,#1760);
#1431=LINE('',#9972,#1761);
#1432=LINE('',#9974,#1762);
#1433=LINE('',#9976,#1763);
#1434=LINE('',#9977,#1764);
#1435=LINE('',#9979,#1765);
#1436=LINE('',#9981,#1766);
#1437=LINE('',#9983,#1767);
#1438=LINE('',#9984,#1768);
#1439=LINE('',#10005,#1769);
#1440=LINE('',#10021,#1770);
#1441=LINE('',#10033,#1771);
#1442=LINE('',#10053,#1772);
#1443=LINE('',#10062,#1773);
#1444=LINE('',#10078,#1774);
#1445=LINE('',#10090,#1775);
#1446=LINE('',#10113,#1776);
#1447=LINE('',#10115,#1777);
#1448=LINE('',#10117,#1778);
#1449=LINE('',#10118,#1779);
#1450=LINE('',#10123,#1780);
#1451=LINE('',#10131,#1781);
#1452=LINE('',#10144,#1782);
#1453=LINE('',#10146,#1783);
#1454=LINE('',#10148,#1784);
#1455=LINE('',#10149,#1785);
#1456=LINE('',#10154,#1786);
#1457=LINE('',#10164,#1787);
#1458=LINE('',#10188,#1788);
#1459=LINE('',#10189,#1789);
#1460=LINE('',#10197,#1790);
#1461=LINE('',#10198,#1791);
#1462=LINE('',#10207,#1792);
#1463=LINE('',#10208,#1793);
#1464=LINE('',#10210,#1794);
#1465=LINE('',#10211,#1795);
#1466=LINE('',#10219,#1796);
#1467=LINE('',#10220,#1797);
#1468=LINE('',#10242,#1798);
#1469=LINE('',#10267,#1799);
#1470=LINE('',#10268,#1800);
#1471=LINE('',#10285,#1801);
#1472=LINE('',#10286,#1802);
#1473=LINE('',#10295,#1803);
#1474=LINE('',#10296,#1804);
#1475=LINE('',#10305,#1805);
#1476=LINE('',#10306,#1806);
#1477=LINE('',#10315,#1807);
#1478=LINE('',#10316,#1808);
#1479=LINE('',#10318,#1809);
#1480=LINE('',#10319,#1810);
#1481=LINE('',#10336,#1811);
#1482=LINE('',#10338,#1812);
#1483=LINE('',#10361,#1813);
#1484=LINE('',#10362,#1814);
#1485=LINE('',#10364,#1815);
#1486=LINE('',#10365,#1816);
#1487=LINE('',#10368,#1817);
#1488=LINE('',#10370,#1818);
#1489=LINE('',#10387,#1819);
#1490=LINE('',#10389,#1820);
#1491=LINE('',#10406,#1821);
#1492=LINE('',#10408,#1822);
#1493=LINE('',#10445,#1823);
#1494=LINE('',#10446,#1824);
#1495=LINE('',#10456,#1825);
#1496=LINE('',#10458,#1826);
#1497=LINE('',#10474,#1827);
#1498=LINE('',#10475,#1828);
#1499=LINE('',#10477,#1829);
#1500=LINE('',#10478,#1830);
#1501=LINE('',#10481,#1831);
#1502=LINE('',#10483,#1832);
#1503=LINE('',#10499,#1833);
#1504=LINE('',#10500,#1834);
#1505=LINE('',#10503,#1835);
#1506=LINE('',#10505,#1836);
#1507=LINE('',#10525,#1837);
#1508=LINE('',#10527,#1838);
#1509=LINE('',#10552,#1839);
#1510=LINE('',#10553,#1840);
#1511=LINE('',#10555,#1841);
#1512=LINE('',#10556,#1842);
#1513=LINE('',#10558,#1843);
#1514=LINE('',#10559,#1844);
#1515=LINE('',#10561,#1845);
#1516=LINE('',#10562,#1846);
#1517=LINE('',#10564,#1847);
#1518=LINE('',#10566,#1848);
#1519=LINE('',#10568,#1849);
#1520=LINE('',#10570,#1850);
#1521=LINE('',#10572,#1851);
#1522=LINE('',#10574,#1852);
#1523=LINE('',#10575,#1853);
#1524=LINE('',#10577,#1854);
#1525=LINE('',#10579,#1855);
#1526=LINE('',#10580,#1856);
#1527=LINE('',#10582,#1857);
#1528=LINE('',#10584,#1858);
#1529=LINE('',#10585,#1859);
#1530=LINE('',#10587,#1860);
#1531=LINE('',#10589,#1861);
#1532=LINE('',#10591,#1862);
#1533=LINE('',#10592,#1863);
#1534=VECTOR('',#6704,4.925);
#1535=VECTOR('',#6709,10.);
#1536=VECTOR('',#6710,10.);
#1537=VECTOR('',#6711,10.);
#1538=VECTOR('',#6712,10.);
#1539=VECTOR('',#6715,10.);
#1540=VECTOR('',#6716,10.);
#1541=VECTOR('',#6717,10.);
#1542=VECTOR('',#6720,10.);
#1543=VECTOR('',#6721,10.);
#1544=VECTOR('',#6722,10.);
#1545=VECTOR('',#6725,10.);
#1546=VECTOR('',#6726,10.);
#1547=VECTOR('',#6741,10.);
#1548=VECTOR('',#6742,10.);
#1549=VECTOR('',#6745,10.);
#1550=VECTOR('',#6746,10.);
#1551=VECTOR('',#6749,10.);
#1552=VECTOR('',#6750,10.);
#1553=VECTOR('',#6751,10.);
#1554=VECTOR('',#6752,10.);
#1555=VECTOR('',#6753,10.);
#1556=VECTOR('',#6754,10.);
#1557=VECTOR('',#6755,10.);
#1558=VECTOR('',#6756,10.);
#1559=VECTOR('',#6757,10.);
#1560=VECTOR('',#6758,10.);
#1561=VECTOR('',#6759,10.);
#1562=VECTOR('',#6762,10.);
#1563=VECTOR('',#6763,10.);
#1564=VECTOR('',#6766,10.);
#1565=VECTOR('',#6767,10.);
#1566=VECTOR('',#6768,10.);
#1567=VECTOR('',#6773,5.);
#1568=VECTOR('',#6788,5.);
#1569=VECTOR('',#6803,10.);
#1570=VECTOR('',#6804,10.);
#1571=VECTOR('',#6805,10.);
#1572=VECTOR('',#6806,10.);
#1573=VECTOR('',#6807,10.);
#1574=VECTOR('',#6810,10.);
#1575=VECTOR('',#6811,10.);
#1576=VECTOR('',#6814,10.);
#1577=VECTOR('',#6815,10.);
#1578=VECTOR('',#6816,10.);
#1579=VECTOR('',#6817,10.);
#1580=VECTOR('',#6818,10.);
#1581=VECTOR('',#6819,10.);
#1582=VECTOR('',#6820,10.);
#1583=VECTOR('',#6821,10.);
#1584=VECTOR('',#6822,10.);
#1585=VECTOR('',#6823,10.);
#1586=VECTOR('',#6824,10.);
#1587=VECTOR('',#6827,10.);
#1588=VECTOR('',#6828,10.);
#1589=VECTOR('',#6845,10.);
#1590=VECTOR('',#6846,10.);
#1591=VECTOR('',#6847,10.);
#1592=VECTOR('',#6848,10.);
#1593=VECTOR('',#6881,1.5);
#1594=VECTOR('',#6892,1.5);
#1595=VECTOR('',#6903,1.5);
#1596=VECTOR('',#6914,1.5);
#1597=VECTOR('',#6925,1.5);
#1598=VECTOR('',#6936,1.5);
#1599=VECTOR('',#6947,1.5);
#1600=VECTOR('',#6960,1.5);
#1601=VECTOR('',#6971,1.5);
#1602=VECTOR('',#6984,1.5);
#1603=VECTOR('',#6995,1.5);
#1604=VECTOR('',#7006,1.5);
#1605=VECTOR('',#7017,1.5);
#1606=VECTOR('',#7028,1.5);
#1607=VECTOR('',#7039,1.5);
#1608=VECTOR('',#7050,1.5);
#1609=VECTOR('',#7057,10.);
#1610=VECTOR('',#7064,10.);
#1611=VECTOR('',#7071,10.);
#1612=VECTOR('',#7076,10.);
#1613=VECTOR('',#7081,10.);
#1614=VECTOR('',#7086,10.);
#1615=VECTOR('',#7089,10.);
#1616=VECTOR('',#7098,10.);
#1617=VECTOR('',#7117,10.);
#1618=VECTOR('',#7118,10.);
#1619=VECTOR('',#7121,10.);
#1620=VECTOR('',#7132,10.);
#1621=VECTOR('',#7153,10.);
#1622=VECTOR('',#7158,10.);
#1623=VECTOR('',#7159,10.);
#1624=VECTOR('',#7170,10.);
#1625=VECTOR('',#7205,10.);
#1626=VECTOR('',#7206,10.);
#1627=VECTOR('',#7209,10.);
#1628=VECTOR('',#7236,10.);
#1629=VECTOR('',#7237,10.);
#1630=VECTOR('',#7248,10.);
#1631=VECTOR('',#7259,10.);
#1632=VECTOR('',#7286,10.);
#1633=VECTOR('',#7287,10.);
#1634=VECTOR('',#7290,10.);
#1635=VECTOR('',#7317,10.);
#1636=VECTOR('',#7318,10.);
#1637=VECTOR('',#7329,10.);
#1638=VECTOR('',#7332,10.);
#1639=VECTOR('',#7351,10.);
#1640=VECTOR('',#7356,10.);
#1641=VECTOR('',#7359,10.);
#1642=VECTOR('',#7364,10.);
#1643=VECTOR('',#7367,10.);
#1644=VECTOR('',#7370,10.);
#1645=VECTOR('',#7373,10.);
#1646=VECTOR('',#7376,10.);
#1647=VECTOR('',#7377,10.);
#1648=VECTOR('',#7380,10.);
#1649=VECTOR('',#7383,10.);
#1650=VECTOR('',#7384,10.);
#1651=VECTOR('',#7387,10.);
#1652=VECTOR('',#7390,10.);
#1653=VECTOR('',#7393,10.);
#1654=VECTOR('',#7396,10.);
#1655=VECTOR('',#7399,10.);
#1656=VECTOR('',#7400,10.);
#1657=VECTOR('',#7403,10.);
#1658=VECTOR('',#7406,10.);
#1659=VECTOR('',#7409,10.);
#1660=VECTOR('',#7410,10.);
#1661=VECTOR('',#7413,10.);
#1662=VECTOR('',#7416,10.);
#1663=VECTOR('',#7419,10.);
#1664=VECTOR('',#7424,10.);
#1665=VECTOR('',#7427,10.);
#1666=VECTOR('',#7432,10.);
#1667=VECTOR('',#7435,10.);
#1668=VECTOR('',#7440,10.);
#1669=VECTOR('',#7443,10.);
#1670=VECTOR('',#7444,10.);
#1671=VECTOR('',#7447,10.);
#1672=VECTOR('',#7450,10.);
#1673=VECTOR('',#7453,10.);
#1674=VECTOR('',#7456,10.);
#1675=VECTOR('',#7459,10.);
#1676=VECTOR('',#7462,10.);
#1677=VECTOR('',#7537,4.);
#1678=VECTOR('',#7552,5.);
#1679=VECTOR('',#7589,4.);
#1680=VECTOR('',#7604,5.);
#1681=VECTOR('',#7635,10.);
#1682=VECTOR('',#7636,10.);
#1683=VECTOR('',#7637,10.);
#1684=VECTOR('',#7638,10.);
#1685=VECTOR('',#7643,1.99999999999999);
#1686=VECTOR('',#7654,1.99999999999999);
#1687=VECTOR('',#7669,10.);
#1688=VECTOR('',#7670,10.);
#1689=VECTOR('',#7671,10.);
#1690=VECTOR('',#7672,10.);
#1691=VECTOR('',#7677,1.99999999999999);
#1692=VECTOR('',#7690,1.99999999999999);
#1693=VECTOR('',#7719,10.);
#1694=VECTOR('',#7720,10.);
#1695=VECTOR('',#7731,10.);
#1696=VECTOR('',#7732,10.);
#1697=VECTOR('',#7743,10.);
#1698=VECTOR('',#7744,10.);
#1699=VECTOR('',#7747,10.);
#1700=VECTOR('',#7748,10.);
#1701=VECTOR('',#7759,10.);
#1702=VECTOR('',#7760,10.);
#1703=VECTOR('',#7789,10.);
#1704=VECTOR('',#7820,10.);
#1705=VECTOR('',#7821,10.);
#1706=VECTOR('',#7842,10.);
#1707=VECTOR('',#7843,10.);
#1708=VECTOR('',#7854,10.);
#1709=VECTOR('',#7855,10.);
#1710=VECTOR('',#7866,10.);
#1711=VECTOR('',#7867,10.);
#1712=VECTOR('',#7878,10.);
#1713=VECTOR('',#7879,10.);
#1714=VECTOR('',#7882,10.);
#1715=VECTOR('',#7883,10.);
#1716=VECTOR('',#7902,10.);
#1717=VECTOR('',#7903,10.);
#1718=VECTOR('',#7914,10.);
#1719=VECTOR('',#7915,10.);
#1720=VECTOR('',#7918,10.);
#1721=VECTOR('',#7919,10.);
#1722=VECTOR('',#7922,10.);
#1723=VECTOR('',#7923,10.);
#1724=VECTOR('',#7926,10.);
#1725=VECTOR('',#7927,10.);
#1726=VECTOR('',#7930,10.);
#1727=VECTOR('',#7931,10.);
#1728=VECTOR('',#7958,10.);
#1729=VECTOR('',#7959,10.);
#1730=VECTOR('',#7970,10.);
#1731=VECTOR('',#7971,10.);
#1732=VECTOR('',#7974,10.);
#1733=VECTOR('',#7975,10.);
#1734=VECTOR('',#7978,10.);
#1735=VECTOR('',#7979,10.);
#1736=VECTOR('',#7982,10.);
#1737=VECTOR('',#7983,10.);
#1738=VECTOR('',#7986,10.);
#1739=VECTOR('',#7987,10.);
#1740=VECTOR('',#7990,10.);
#1741=VECTOR('',#7991,10.);
#1742=VECTOR('',#8000,10.);
#1743=VECTOR('',#8001,10.);
#1744=VECTOR('',#8022,10.);
#1745=VECTOR('',#8023,10.);
#1746=VECTOR('',#8026,10.);
#1747=VECTOR('',#8027,10.);
#1748=VECTOR('',#8030,10.);
#1749=VECTOR('',#8031,10.);
#1750=VECTOR('',#8034,10.);
#1751=VECTOR('',#8035,10.);
#1752=VECTOR('',#8038,10.);
#1753=VECTOR('',#8041,10.);
#1754=VECTOR('',#8044,10.);
#1755=VECTOR('',#8047,10.);
#1756=VECTOR('',#8050,10.);
#1757=VECTOR('',#8053,10.);
#1758=VECTOR('',#8054,10.);
#1759=VECTOR('',#8057,10.);
#1760=VECTOR('',#8060,10.);
#1761=VECTOR('',#8061,10.);
#1762=VECTOR('',#8064,10.);
#1763=VECTOR('',#8067,10.);
#1764=VECTOR('',#8068,10.);
#1765=VECTOR('',#8071,10.);
#1766=VECTOR('',#8074,10.);
#1767=VECTOR('',#8077,10.);
#1768=VECTOR('',#8078,10.);
#1769=VECTOR('',#8115,5.);
#1770=VECTOR('',#8136,4.);
#1771=VECTOR('',#8151,5.);
#1772=VECTOR('',#8180,4.);
#1773=VECTOR('',#8193,4.);
#1774=VECTOR('',#8214,4.);
#1775=VECTOR('',#8229,5.);
#1776=VECTOR('',#8260,10.);
#1777=VECTOR('',#8261,10.);
#1778=VECTOR('',#8262,10.);
#1779=VECTOR('',#8263,10.);
#1780=VECTOR('',#8268,1.99999999999999);
#1781=VECTOR('',#8279,1.99999999999999);
#1782=VECTOR('',#8294,10.);
#1783=VECTOR('',#8295,10.);
#1784=VECTOR('',#8296,10.);
#1785=VECTOR('',#8297,10.);
#1786=VECTOR('',#8302,1.99999999999999);
#1787=VECTOR('',#8315,1.99999999999999);
#1788=VECTOR('',#8344,10.);
#1789=VECTOR('',#8345,10.);
#1790=VECTOR('',#8356,10.);
#1791=VECTOR('',#8357,10.);
#1792=VECTOR('',#8368,10.);
#1793=VECTOR('',#8369,10.);
#1794=VECTOR('',#8372,10.);
#1795=VECTOR('',#8373,10.);
#1796=VECTOR('',#8384,10.);
#1797=VECTOR('',#8385,10.);
#1798=VECTOR('',#8414,10.);
#1799=VECTOR('',#8445,10.);
#1800=VECTOR('',#8446,10.);
#1801=VECTOR('',#8467,10.);
#1802=VECTOR('',#8468,10.);
#1803=VECTOR('',#8479,10.);
#1804=VECTOR('',#8480,10.);
#1805=VECTOR('',#8491,10.);
#1806=VECTOR('',#8492,10.);
#1807=VECTOR('',#8503,10.);
#1808=VECTOR('',#8504,10.);
#1809=VECTOR('',#8507,10.);
#1810=VECTOR('',#8508,10.);
#1811=VECTOR('',#8527,10.);
#1812=VECTOR('',#8528,10.);
#1813=VECTOR('',#8539,10.);
#1814=VECTOR('',#8540,10.);
#1815=VECTOR('',#8543,10.);
#1816=VECTOR('',#8544,10.);
#1817=VECTOR('',#8547,10.);
#1818=VECTOR('',#8548,10.);
#1819=VECTOR('',#8551,10.);
#1820=VECTOR('',#8552,10.);
#1821=VECTOR('',#8555,10.);
#1822=VECTOR('',#8556,10.);
#1823=VECTOR('',#8583,10.);
#1824=VECTOR('',#8584,10.);
#1825=VECTOR('',#8595,10.);
#1826=VECTOR('',#8596,10.);
#1827=VECTOR('',#8599,10.);
#1828=VECTOR('',#8600,10.);
#1829=VECTOR('',#8603,10.);
#1830=VECTOR('',#8604,10.);
#1831=VECTOR('',#8607,10.);
#1832=VECTOR('',#8608,10.);
#1833=VECTOR('',#8611,10.);
#1834=VECTOR('',#8612,10.);
#1835=VECTOR('',#8615,10.);
#1836=VECTOR('',#8616,10.);
#1837=VECTOR('',#8625,10.);
#1838=VECTOR('',#8626,10.);
#1839=VECTOR('',#8647,10.);
#1840=VECTOR('',#8648,10.);
#1841=VECTOR('',#8651,10.);
#1842=VECTOR('',#8652,10.);
#1843=VECTOR('',#8655,10.);
#1844=VECTOR('',#8656,10.);
#1845=VECTOR('',#8659,10.);
#1846=VECTOR('',#8660,10.);
#1847=VECTOR('',#8663,10.);
#1848=VECTOR('',#8666,10.);
#1849=VECTOR('',#8669,10.);
#1850=VECTOR('',#8672,10.);
#1851=VECTOR('',#8675,10.);
#1852=VECTOR('',#8678,10.);
#1853=VECTOR('',#8679,10.);
#1854=VECTOR('',#8682,10.);
#1855=VECTOR('',#8685,10.);
#1856=VECTOR('',#8686,10.);
#1857=VECTOR('',#8689,10.);
#1858=VECTOR('',#8692,10.);
#1859=VECTOR('',#8693,10.);
#1860=VECTOR('',#8696,10.);
#1861=VECTOR('',#8699,10.);
#1862=VECTOR('',#8702,10.);
#1863=VECTOR('',#8703,10.);
#1864=CIRCLE('',#5837,5.13675);
#1865=CIRCLE('',#5838,5.13675);
#1866=CIRCLE('',#5845,5.3);
#1867=CIRCLE('',#5846,0.3);
#1868=CIRCLE('',#5847,5.);
#1869=CIRCLE('',#5848,5.);
#1870=CIRCLE('',#5850,0.599999999999996);
#1871=CIRCLE('',#5851,0.599999999999996);
#1872=CIRCLE('',#5852,0.600000000000001);
#1873=CIRCLE('',#5853,0.600000000000001);
#1874=CIRCLE('',#5854,5.3);
#1875=CIRCLE('',#5856,5.);
#1876=CIRCLE('',#5857,5.);
#1877=CIRCLE('',#5859,5.);
#1878=CIRCLE('',#5860,0.3);
#1879=CIRCLE('',#5861,5.);
#1880=CIRCLE('',#5863,5.);
#1881=CIRCLE('',#5864,5.);
#1882=CIRCLE('',#5866,5.3);
#1883=CIRCLE('',#5867,0.3);
#1884=CIRCLE('',#5869,0.600000000000001);
#1885=CIRCLE('',#5870,0.600000000000001);
#1886=CIRCLE('',#5871,0.599999999999996);
#1887=CIRCLE('',#5872,0.600000000000001);
#1888=CIRCLE('',#5873,5.3);
#1889=CIRCLE('',#5875,0.3);
#1890=CIRCLE('',#5877,1.8);
#1891=CIRCLE('',#5878,0.3);
#1892=CIRCLE('',#5879,1.5);
#1893=CIRCLE('',#5881,1.8);
#1894=CIRCLE('',#5882,1.8);
#1895=CIRCLE('',#5883,1.8);
#1896=CIRCLE('',#5884,1.8);
#1897=CIRCLE('',#5885,1.8);
#1898=CIRCLE('',#5886,1.8);
#1899=CIRCLE('',#5887,1.8);
#1900=CIRCLE('',#5888,1.8);
#1901=CIRCLE('',#5889,1.8);
#1902=CIRCLE('',#5890,1.8);
#1903=CIRCLE('',#5891,1.8);
#1904=CIRCLE('',#5892,1.8);
#1905=CIRCLE('',#5893,1.8);
#1906=CIRCLE('',#5894,1.8);
#1907=CIRCLE('',#5895,1.8);
#1908=CIRCLE('',#5897,1.5);
#1909=CIRCLE('',#5899,0.3);
#1910=CIRCLE('',#5900,1.5);
#1911=CIRCLE('',#5902,1.5);
#1912=CIRCLE('',#5904,0.3);
#1913=CIRCLE('',#5905,1.5);
#1914=CIRCLE('',#5907,1.5);
#1915=CIRCLE('',#5909,0.3);
#1916=CIRCLE('',#5910,1.5);
#1917=CIRCLE('',#5912,1.5);
#1918=CIRCLE('',#5914,0.3);
#1919=CIRCLE('',#5915,1.5);
#1920=CIRCLE('',#5917,1.5);
#1921=CIRCLE('',#5919,0.3);
#1922=CIRCLE('',#5920,1.5);
#1923=CIRCLE('',#5922,1.5);
#1924=CIRCLE('',#5924,0.3);
#1925=CIRCLE('',#5925,1.5);
#1926=CIRCLE('',#5927,1.5);
#1927=CIRCLE('',#5929,0.3);
#1928=CIRCLE('',#5930,1.5);
#1929=CIRCLE('',#5931,1.5);
#1930=CIRCLE('',#5933,1.5);
#1931=CIRCLE('',#5935,0.3);
#1932=CIRCLE('',#5936,1.5);
#1933=CIRCLE('',#5938,1.5);
#1934=CIRCLE('',#5940,0.3);
#1935=CIRCLE('',#5941,1.5);
#1936=CIRCLE('',#5942,1.5);
#1937=CIRCLE('',#5944,1.5);
#1938=CIRCLE('',#5946,0.3);
#1939=CIRCLE('',#5947,1.5);
#1940=CIRCLE('',#5949,1.5);
#1941=CIRCLE('',#5951,0.3);
#1942=CIRCLE('',#5952,1.5);
#1943=CIRCLE('',#5954,1.5);
#1944=CIRCLE('',#5956,0.3);
#1945=CIRCLE('',#5957,1.5);
#1946=CIRCLE('',#5959,1.5);
#1947=CIRCLE('',#5961,0.3);
#1948=CIRCLE('',#5962,1.5);
#1949=CIRCLE('',#5964,1.5);
#1950=CIRCLE('',#5966,0.3);
#1951=CIRCLE('',#5967,1.5);
#1952=CIRCLE('',#5969,1.5);
#1953=CIRCLE('',#5971,0.3);
#1954=CIRCLE('',#5972,1.5);
#1955=CIRCLE('',#5974,1.5);
#1956=CIRCLE('',#5995,0.3);
#1957=CIRCLE('',#5996,0.299999999999998);
#1958=CIRCLE('',#5997,0.299999999999998);
#1959=CIRCLE('',#5999,0.299999999999998);
#1960=CIRCLE('',#6000,0.3);
#1961=CIRCLE('',#6001,0.299999999999998);
#1962=CIRCLE('',#6005,0.3);
#1963=CIRCLE('',#6006,0.299999999999998);
#1964=CIRCLE('',#6007,0.299999999999998);
#1965=CIRCLE('',#6011,0.3);
#1966=CIRCLE('',#6012,0.299999999999998);
#1967=CIRCLE('',#6013,0.299999999999998);
#1968=CIRCLE('',#6015,0.299999999999998);
#1969=CIRCLE('',#6016,0.3);
#1970=CIRCLE('',#6017,0.299999999999998);
#1971=CIRCLE('',#6022,0.299999999999998);
#1972=CIRCLE('',#6023,0.299999999999998);
#1973=CIRCLE('',#6024,0.3);
#1974=CIRCLE('',#6027,0.3);
#1975=CIRCLE('',#6028,0.299999999999998);
#1976=CIRCLE('',#6029,0.299999999999998);
#1977=CIRCLE('',#6031,0.3);
#1978=CIRCLE('',#6032,0.299999999999998);
#1979=CIRCLE('',#6033,0.299999999999998);
#1980=CIRCLE('',#6035,0.3);
#1981=CIRCLE('',#6036,0.299999999999998);
#1982=CIRCLE('',#6037,0.299999999999998);
#1983=CIRCLE('',#6039,0.299999999999998);
#1984=CIRCLE('',#6040,0.3);
#1985=CIRCLE('',#6041,0.299999999999998);
#1986=CIRCLE('',#6045,0.299999999999998);
#1987=CIRCLE('',#6046,0.3);
#1988=CIRCLE('',#6047,0.299999999999998);
#1989=CIRCLE('',#6049,0.3);
#1990=CIRCLE('',#6050,0.299999999999998);
#1991=CIRCLE('',#6051,0.299999999999998);
#1992=CIRCLE('',#6053,0.3);
#1993=CIRCLE('',#6054,0.299999999999994);
#1994=CIRCLE('',#6055,0.299999999999998);
#1995=CIRCLE('',#6058,0.299999999999998);
#1996=CIRCLE('',#6059,0.299999999999998);
#1997=CIRCLE('',#6060,0.3);
#1998=CIRCLE('',#6063,0.299999999999998);
#1999=CIRCLE('',#6064,0.299999999999998);
#2000=CIRCLE('',#6065,0.3);
#2001=CIRCLE('',#6068,0.3);
#2002=CIRCLE('',#6069,0.299999999999998);
#2003=CIRCLE('',#6070,0.299999999999998);
#2004=CIRCLE('',#6072,0.3);
#2005=CIRCLE('',#6073,0.299999999999998);
#2006=CIRCLE('',#6074,0.299999999999998);
#2007=CIRCLE('',#6076,0.299999999999998);
#2008=CIRCLE('',#6077,0.3);
#2009=CIRCLE('',#6078,0.299999999999998);
#2010=CIRCLE('',#6082,0.299999999999998);
#2011=CIRCLE('',#6083,0.3);
#2012=CIRCLE('',#6084,0.299999999999998);
#2013=CIRCLE('',#6086,0.299999999999998);
#2014=CIRCLE('',#6087,0.3);
#2015=CIRCLE('',#6088,0.299999999999998);
#2016=CIRCLE('',#6090,0.3);
#2017=CIRCLE('',#6091,0.299999999999998);
#2018=CIRCLE('',#6092,0.299999999999998);
#2019=CIRCLE('',#6095,0.3);
#2020=CIRCLE('',#6096,0.299999999999998);
#2021=CIRCLE('',#6097,0.299999999999998);
#2022=CIRCLE('',#6101,0.3);
#2023=CIRCLE('',#6102,0.299999999999998);
#2024=CIRCLE('',#6103,0.299999999999998);
#2025=CIRCLE('',#6105,0.299999999999998);
#2026=CIRCLE('',#6106,0.300000000000002);
#2027=CIRCLE('',#6107,0.299999999999998);
#2028=CIRCLE('',#6176,4.3);
#2029=CIRCLE('',#6177,0.3);
#2030=CIRCLE('',#6178,4.);
#2031=CIRCLE('',#6179,4.);
#2032=CIRCLE('',#6181,4.7);
#2033=CIRCLE('',#6183,4.);
#2034=CIRCLE('',#6184,4.);
#2035=CIRCLE('',#6186,0.3);
#2036=CIRCLE('',#6187,5.);
#2037=CIRCLE('',#6188,5.);
#2038=CIRCLE('',#6190,5.);
#2039=CIRCLE('',#6191,5.);
#2040=CIRCLE('',#6193,4.3);
#2041=CIRCLE('',#6194,0.3);
#2042=CIRCLE('',#6196,4.7);
#2043=CIRCLE('',#6198,0.3);
#2044=CIRCLE('',#6201,4.3);
#2045=CIRCLE('',#6202,0.3);
#2046=CIRCLE('',#6203,4.);
#2047=CIRCLE('',#6204,4.);
#2048=CIRCLE('',#6206,4.7);
#2049=CIRCLE('',#6208,4.);
#2050=CIRCLE('',#6209,4.);
#2051=CIRCLE('',#6211,0.3);
#2052=CIRCLE('',#6212,5.);
#2053=CIRCLE('',#6213,5.);
#2054=CIRCLE('',#6215,5.);
#2055=CIRCLE('',#6216,5.);
#2056=CIRCLE('',#6218,4.3);
#2057=CIRCLE('',#6219,0.3);
#2058=CIRCLE('',#6221,4.7);
#2059=CIRCLE('',#6223,0.3);
#2060=CIRCLE('',#6226,1.99999999999999);
#2061=CIRCLE('',#6227,0.3);
#2062=CIRCLE('',#6228,2.29999999999999);
#2063=CIRCLE('',#6230,2.29999999999999);
#2064=CIRCLE('',#6232,1.99999999999999);
#2065=CIRCLE('',#6234,1.99999999999999);
#2066=CIRCLE('',#6235,0.3);
#2067=CIRCLE('',#6237,1.99999999999999);
#2068=CIRCLE('',#6239,2.29999999999999);
#2069=CIRCLE('',#6240,0.3);
#2070=CIRCLE('',#6241,1.99999999999999);
#2071=CIRCLE('',#6242,1.99999999999999);
#2072=CIRCLE('',#6244,2.29999999999999);
#2073=CIRCLE('',#6246,1.99999999999999);
#2074=CIRCLE('',#6248,0.3);
#2075=CIRCLE('',#6249,1.99999999999999);
#2076=CIRCLE('',#6250,1.99999999999999);
#2077=CIRCLE('',#6252,1.99999999999999);
#2078=CIRCLE('',#6254,0.299999999999994);
#2079=CIRCLE('',#6255,0.299999999999998);
#2080=CIRCLE('',#6256,0.3);
#2081=CIRCLE('',#6258,0.300000000000002);
#2082=CIRCLE('',#6259,0.299999999999994);
#2083=CIRCLE('',#6260,0.299999999999994);
#2084=CIRCLE('',#6262,0.3);
#2085=CIRCLE('',#6263,0.299999999999998);
#2086=CIRCLE('',#6264,0.300000000000011);
#2087=CIRCLE('',#6267,0.299999999999994);
#2088=CIRCLE('',#6268,0.299999999999998);
#2089=CIRCLE('',#6269,0.299999999999998);
#2090=CIRCLE('',#6272,0.299999999999994);
#2091=CIRCLE('',#6273,0.299999999999998);
#2092=CIRCLE('',#6274,0.3);
#2093=CIRCLE('',#6278,0.299999999999998);
#2094=CIRCLE('',#6279,0.3);
#2095=CIRCLE('',#6280,0.299999999999994);
#2096=CIRCLE('',#6283,0.299999999999994);
#2097=CIRCLE('',#6284,0.299999999999994);
#2098=CIRCLE('',#6285,0.3);
#2099=CIRCLE('',#6287,0.299999999999998);
#2100=CIRCLE('',#6288,0.3);
#2101=CIRCLE('',#6289,0.599999999999996);
#2102=CIRCLE('',#6290,0.299999999999994);
#2103=CIRCLE('',#6292,0.299999999999994);
#2104=CIRCLE('',#6293,0.299999999999994);
#2105=CIRCLE('',#6294,0.3);
#2106=CIRCLE('',#6297,0.600000000000001);
#2107=CIRCLE('',#6298,0.299999999999994);
#2108=CIRCLE('',#6299,0.3);
#2109=CIRCLE('',#6300,0.299999999999998);
#2110=CIRCLE('',#6302,0.600000000000001);
#2111=CIRCLE('',#6303,0.299999999999976);
#2112=CIRCLE('',#6304,0.3);
#2113=CIRCLE('',#6305,0.299999999999994);
#2114=CIRCLE('',#6307,0.300000000000011);
#2115=CIRCLE('',#6308,0.3);
#2116=CIRCLE('',#6309,0.299999999999998);
#2117=CIRCLE('',#6312,0.299999999999994);
#2118=CIRCLE('',#6313,0.3);
#2119=CIRCLE('',#6314,0.599999999999987);
#2120=CIRCLE('',#6315,0.299999999999994);
#2121=CIRCLE('',#6317,0.299999999999998);
#2122=CIRCLE('',#6318,0.3);
#2123=CIRCLE('',#6319,0.299999999999994);
#2124=CIRCLE('',#6322,0.300000000000002);
#2125=CIRCLE('',#6323,0.3);
#2126=CIRCLE('',#6324,0.299999999999994);
#2127=CIRCLE('',#6327,0.299999999999994);
#2128=CIRCLE('',#6328,0.299999999999998);
#2129=CIRCLE('',#6329,0.3);
#2130=CIRCLE('',#6332,0.299999999999994);
#2131=CIRCLE('',#6333,0.3);
#2132=CIRCLE('',#6334,0.299999999999994);
#2133=CIRCLE('',#6338,0.299999999999994);
#2134=CIRCLE('',#6339,0.300000000000002);
#2135=CIRCLE('',#6340,0.299999999999998);
#2136=CIRCLE('',#6342,0.299999999999998);
#2137=CIRCLE('',#6343,0.300000000000011);
#2138=CIRCLE('',#6344,0.300000000000002);
#2139=CIRCLE('',#6347,0.299999999999994);
#2140=CIRCLE('',#6348,0.299999999999998);
#2141=CIRCLE('',#6349,0.3);
#2142=CIRCLE('',#6356,0.299999999999998);
#2143=CIRCLE('',#6357,0.300000000000011);
#2144=CIRCLE('',#6358,0.3);
#2145=CIRCLE('',#6360,0.299999999999994);
#2146=CIRCLE('',#6361,0.299999999999998);
#2147=CIRCLE('',#6362,0.3);
#2148=CIRCLE('',#6364,0.299999999999994);
#2149=CIRCLE('',#6365,0.299999999999998);
#2150=CIRCLE('',#6366,0.3);
#2151=CIRCLE('',#6369,0.299999999999994);
#2152=CIRCLE('',#6370,0.3);
#2153=CIRCLE('',#6371,0.299999999999994);
#2154=CIRCLE('',#6379,4.);
#2155=CIRCLE('',#6380,4.3);
#2156=CIRCLE('',#6383,4.3);
#2157=CIRCLE('',#6384,4.);
#2158=CIRCLE('',#6386,4.3);
#2159=CIRCLE('',#6387,4.);
#2160=CIRCLE('',#6389,4.);
#2161=CIRCLE('',#6390,4.3);
#2162=CIRCLE('',#6423,4.925);
#2163=CIRCLE('',#6425,4.925);
#2164=CIRCLE('',#6429,4.3);
#2165=CIRCLE('',#6430,0.3);
#2166=CIRCLE('',#6431,4.);
#2167=CIRCLE('',#6432,4.);
#2168=CIRCLE('',#6434,4.7);
#2169=CIRCLE('',#6436,4.);
#2170=CIRCLE('',#6437,4.);
#2171=CIRCLE('',#6439,0.3);
#2172=CIRCLE('',#6440,5.);
#2173=CIRCLE('',#6441,5.);
#2174=CIRCLE('',#6443,5.);
#2175=CIRCLE('',#6444,5.);
#2176=CIRCLE('',#6446,4.3);
#2177=CIRCLE('',#6447,0.3);
#2178=CIRCLE('',#6449,4.7);
#2179=CIRCLE('',#6451,0.3);
#2180=CIRCLE('',#6454,4.);
#2181=CIRCLE('',#6456,4.);
#2182=CIRCLE('',#6460,4.);
#2183=CIRCLE('',#6462,4.);
#2184=CIRCLE('',#6466,4.3);
#2185=CIRCLE('',#6467,0.3);
#2186=CIRCLE('',#6468,4.);
#2187=CIRCLE('',#6469,4.);
#2188=CIRCLE('',#6471,4.7);
#2189=CIRCLE('',#6473,4.);
#2190=CIRCLE('',#6474,4.);
#2191=CIRCLE('',#6476,0.3);
#2192=CIRCLE('',#6477,5.);
#2193=CIRCLE('',#6478,5.);
#2194=CIRCLE('',#6480,5.);
#2195=CIRCLE('',#6481,5.);
#2196=CIRCLE('',#6483,4.3);
#2197=CIRCLE('',#6484,0.3);
#2198=CIRCLE('',#6486,4.7);
#2199=CIRCLE('',#6488,0.3);
#2200=CIRCLE('',#6491,1.99999999999999);
#2201=CIRCLE('',#6492,0.3);
#2202=CIRCLE('',#6493,2.29999999999999);
#2203=CIRCLE('',#6495,2.29999999999999);
#2204=CIRCLE('',#6497,1.99999999999999);
#2205=CIRCLE('',#6499,1.99999999999999);
#2206=CIRCLE('',#6500,0.3);
#2207=CIRCLE('',#6502,1.99999999999999);
#2208=CIRCLE('',#6504,2.29999999999999);
#2209=CIRCLE('',#6505,0.3);
#2210=CIRCLE('',#6506,1.99999999999999);
#2211=CIRCLE('',#6507,1.99999999999999);
#2212=CIRCLE('',#6509,2.29999999999999);
#2213=CIRCLE('',#6511,1.99999999999999);
#2214=CIRCLE('',#6513,0.3);
#2215=CIRCLE('',#6514,1.99999999999999);
#2216=CIRCLE('',#6515,1.99999999999999);
#2217=CIRCLE('',#6517,1.99999999999999);
#2218=CIRCLE('',#6519,0.299999999999994);
#2219=CIRCLE('',#6520,0.3);
#2220=CIRCLE('',#6521,0.299999999999998);
#2221=CIRCLE('',#6523,0.300000000000002);
#2222=CIRCLE('',#6524,0.299999999999994);
#2223=CIRCLE('',#6525,0.299999999999994);
#2224=CIRCLE('',#6527,0.3);
#2225=CIRCLE('',#6528,0.300000000000011);
#2226=CIRCLE('',#6529,0.299999999999998);
#2227=CIRCLE('',#6532,0.299999999999994);
#2228=CIRCLE('',#6533,0.299999999999998);
#2229=CIRCLE('',#6534,0.299999999999998);
#2230=CIRCLE('',#6537,0.299999999999994);
#2231=CIRCLE('',#6538,0.3);
#2232=CIRCLE('',#6539,0.299999999999998);
#2233=CIRCLE('',#6543,0.299999999999998);
#2234=CIRCLE('',#6544,0.299999999999994);
#2235=CIRCLE('',#6545,0.3);
#2236=CIRCLE('',#6548,0.299999999999994);
#2237=CIRCLE('',#6549,0.3);
#2238=CIRCLE('',#6550,0.299999999999994);
#2239=CIRCLE('',#6552,0.299999999999998);
#2240=CIRCLE('',#6553,0.299999999999994);
#2241=CIRCLE('',#6554,0.599999999999996);
#2242=CIRCLE('',#6555,0.3);
#2243=CIRCLE('',#6557,0.299999999999994);
#2244=CIRCLE('',#6558,0.3);
#2245=CIRCLE('',#6559,0.299999999999994);
#2246=CIRCLE('',#6562,0.600000000000001);
#2247=CIRCLE('',#6563,0.299999999999998);
#2248=CIRCLE('',#6564,0.3);
#2249=CIRCLE('',#6565,0.299999999999994);
#2250=CIRCLE('',#6567,0.600000000000001);
#2251=CIRCLE('',#6568,0.299999999999994);
#2252=CIRCLE('',#6569,0.3);
#2253=CIRCLE('',#6570,0.299999999999976);
#2254=CIRCLE('',#6572,0.300000000000011);
#2255=CIRCLE('',#6573,0.299999999999998);
#2256=CIRCLE('',#6574,0.3);
#2257=CIRCLE('',#6577,0.299999999999994);
#2258=CIRCLE('',#6578,0.299999999999994);
#2259=CIRCLE('',#6579,0.599999999999987);
#2260=CIRCLE('',#6580,0.3);
#2261=CIRCLE('',#6582,0.299999999999998);
#2262=CIRCLE('',#6583,0.299999999999994);
#2263=CIRCLE('',#6584,0.3);
#2264=CIRCLE('',#6587,0.300000000000002);
#2265=CIRCLE('',#6588,0.299999999999994);
#2266=CIRCLE('',#6589,0.3);
#2267=CIRCLE('',#6592,0.299999999999994);
#2268=CIRCLE('',#6593,0.3);
#2269=CIRCLE('',#6594,0.299999999999998);
#2270=CIRCLE('',#6597,0.299999999999994);
#2271=CIRCLE('',#6598,0.299999999999994);
#2272=CIRCLE('',#6599,0.3);
#2273=CIRCLE('',#6603,0.299999999999994);
#2274=CIRCLE('',#6604,0.299999999999998);
#2275=CIRCLE('',#6605,0.300000000000002);
#2276=CIRCLE('',#6607,0.299999999999998);
#2277=CIRCLE('',#6608,0.300000000000002);
#2278=CIRCLE('',#6609,0.300000000000011);
#2279=CIRCLE('',#6612,0.299999999999994);
#2280=CIRCLE('',#6613,0.3);
#2281=CIRCLE('',#6614,0.299999999999998);
#2282=CIRCLE('',#6621,0.299999999999998);
#2283=CIRCLE('',#6622,0.3);
#2284=CIRCLE('',#6623,0.300000000000011);
#2285=CIRCLE('',#6625,0.299999999999994);
#2286=CIRCLE('',#6626,0.3);
#2287=CIRCLE('',#6627,0.299999999999998);
#2288=CIRCLE('',#6629,0.299999999999994);
#2289=CIRCLE('',#6630,0.3);
#2290=CIRCLE('',#6631,0.299999999999998);
#2291=CIRCLE('',#6634,0.299999999999994);
#2292=CIRCLE('',#6635,0.299999999999994);
#2293=CIRCLE('',#6636,0.3);
#2294=CIRCLE('',#6644,4.);
#2295=CIRCLE('',#6645,4.3);
#2296=CIRCLE('',#6648,4.3);
#2297=CIRCLE('',#6649,4.);
#2298=CIRCLE('',#6651,4.3);
#2299=CIRCLE('',#6652,4.);
#2300=CIRCLE('',#6654,4.);
#2301=CIRCLE('',#6655,4.3);
#2302=VERTEX_POINT('',#8753);
#2303=VERTEX_POINT('',#8755);
#2304=VERTEX_POINT('',#8759);
#2305=VERTEX_POINT('',#8760);
#2306=VERTEX_POINT('',#8762);
#2307=VERTEX_POINT('',#8764);
#2308=VERTEX_POINT('',#8768);
#2309=VERTEX_POINT('',#8770);
#2310=VERTEX_POINT('',#8774);
#2311=VERTEX_POINT('',#8776);
#2312=VERTEX_POINT('',#8784);
#2313=VERTEX_POINT('',#8786);
#2314=VERTEX_POINT('',#8788);
#2315=VERTEX_POINT('',#8792);
#2316=VERTEX_POINT('',#8793);
#2317=VERTEX_POINT('',#8795);
#2318=VERTEX_POINT('',#8797);
#2319=VERTEX_POINT('',#8799);
#2320=VERTEX_POINT('',#8801);
#2321=VERTEX_POINT('',#8803);
#2322=VERTEX_POINT('',#8805);
#2323=VERTEX_POINT('',#8807);
#2324=VERTEX_POINT('',#8809);
#2325=VERTEX_POINT('',#8811);
#2326=VERTEX_POINT('',#8813);
#2327=VERTEX_POINT('',#8815);
#2328=VERTEX_POINT('',#8817);
#2329=VERTEX_POINT('',#8819);
#2330=VERTEX_POINT('',#8821);
#2331=VERTEX_POINT('',#8823);
#2332=VERTEX_POINT('',#8825);
#2333=VERTEX_POINT('',#8827);
#2334=VERTEX_POINT('',#8829);
#2335=VERTEX_POINT('',#8831);
#2336=VERTEX_POINT('',#8833);
#2337=VERTEX_POINT('',#8835);
#2338=VERTEX_POINT('',#8837);
#2339=VERTEX_POINT('',#8840);
#2340=VERTEX_POINT('',#8843);
#2341=VERTEX_POINT('',#8845);
#2342=VERTEX_POINT('',#8849);
#2343=VERTEX_POINT('',#8850);
#2344=VERTEX_POINT('',#8855);
#2345=VERTEX_POINT('',#8857);
#2346=VERTEX_POINT('',#8861);
#2347=VERTEX_POINT('',#8865);
#2348=VERTEX_POINT('',#8866);
#2349=VERTEX_POINT('',#8868);
#2350=VERTEX_POINT('',#8870);
#2351=VERTEX_POINT('',#8872);
#2352=VERTEX_POINT('',#8874);
#2353=VERTEX_POINT('',#8876);
#2354=VERTEX_POINT('',#8878);
#2355=VERTEX_POINT('',#8880);
#2356=VERTEX_POINT('',#8882);
#2357=VERTEX_POINT('',#8884);
#2358=VERTEX_POINT('',#8886);
#2359=VERTEX_POINT('',#8888);
#2360=VERTEX_POINT('',#8890);
#2361=VERTEX_POINT('',#8892);
#2362=VERTEX_POINT('',#8894);
#2363=VERTEX_POINT('',#8896);
#2364=VERTEX_POINT('',#8898);
#2365=VERTEX_POINT('',#8900);
#2366=VERTEX_POINT('',#8902);
#2367=VERTEX_POINT('',#8904);
#2368=VERTEX_POINT('',#8906);
#2369=VERTEX_POINT('',#8908);
#2370=VERTEX_POINT('',#8910);
#2371=VERTEX_POINT('',#8913);
#2372=VERTEX_POINT('',#8918);
#2373=VERTEX_POINT('',#8920);
#2374=VERTEX_POINT('',#8924);
#2375=VERTEX_POINT('',#8925);
#2376=VERTEX_POINT('',#8927);
#2377=VERTEX_POINT('',#8929);
#2378=VERTEX_POINT('',#8932);
#2379=VERTEX_POINT('',#8934);
#2380=VERTEX_POINT('',#8936);
#2381=VERTEX_POINT('',#8938);
#2382=VERTEX_POINT('',#8940);
#2383=VERTEX_POINT('',#8942);
#2384=VERTEX_POINT('',#8944);
#2385=VERTEX_POINT('',#8946);
#2386=VERTEX_POINT('',#8948);
#2387=VERTEX_POINT('',#8950);
#2388=VERTEX_POINT('',#8952);
#2389=VERTEX_POINT('',#8954);
#2390=VERTEX_POINT('',#8956);
#2391=VERTEX_POINT('',#8958);
#2392=VERTEX_POINT('',#8960);
#2393=VERTEX_POINT('',#8963);
#2394=VERTEX_POINT('',#8967);
#2395=VERTEX_POINT('',#8971);
#2396=VERTEX_POINT('',#8975);
#2397=VERTEX_POINT('',#8979);
#2398=VERTEX_POINT('',#8983);
#2399=VERTEX_POINT('',#8987);
#2400=VERTEX_POINT('',#8991);
#2401=VERTEX_POINT('',#8995);
#2402=VERTEX_POINT('',#8999);
#2403=VERTEX_POINT('',#9003);
#2404=VERTEX_POINT('',#9007);
#2405=VERTEX_POINT('',#9011);
#2406=VERTEX_POINT('',#9015);
#2407=VERTEX_POINT('',#9017);
#2408=VERTEX_POINT('',#9021);
#2409=VERTEX_POINT('',#9025);
#2410=VERTEX_POINT('',#9029);
#2411=VERTEX_POINT('',#9033);
#2412=VERTEX_POINT('',#9035);
#2413=VERTEX_POINT('',#9039);
#2414=VERTEX_POINT('',#9043);
#2415=VERTEX_POINT('',#9047);
#2416=VERTEX_POINT('',#9051);
#2417=VERTEX_POINT('',#9055);
#2418=VERTEX_POINT('',#9059);
#2419=VERTEX_POINT('',#9063);
#2420=VERTEX_POINT('',#9067);
#2421=VERTEX_POINT('',#9071);
#2422=VERTEX_POINT('',#9075);
#2423=VERTEX_POINT('',#9079);
#2424=VERTEX_POINT('',#9083);
#2425=VERTEX_POINT('',#9087);
#2426=VERTEX_POINT('',#9091);
#2427=VERTEX_POINT('',#9093);
#2428=VERTEX_POINT('',#9097);
#2429=VERTEX_POINT('',#9099);
#2430=VERTEX_POINT('',#9103);
#2431=VERTEX_POINT('',#9107);
#2432=VERTEX_POINT('',#9111);
#2433=VERTEX_POINT('',#9115);
#2434=VERTEX_POINT('',#9119);
#2435=VERTEX_POINT('',#9120);
#2436=VERTEX_POINT('',#9125);
#2437=VERTEX_POINT('',#9129);
#2438=VERTEX_POINT('',#9131);
#2439=VERTEX_POINT('',#9135);
#2440=VERTEX_POINT('',#9137);
#2441=VERTEX_POINT('',#9146);
#2442=VERTEX_POINT('',#9147);
#2443=VERTEX_POINT('',#9152);
#2444=VERTEX_POINT('',#9156);
#2445=VERTEX_POINT('',#9157);
#2446=VERTEX_POINT('',#9162);
#2447=VERTEX_POINT('',#9164);
#2448=VERTEX_POINT('',#9168);
#2449=VERTEX_POINT('',#9175);
#2450=VERTEX_POINT('',#9176);
#2451=VERTEX_POINT('',#9183);
#2452=VERTEX_POINT('',#9185);
#2453=VERTEX_POINT('',#9189);
#2454=VERTEX_POINT('',#9191);
#2455=VERTEX_POINT('',#9195);
#2456=VERTEX_POINT('',#9196);
#2457=VERTEX_POINT('',#9201);
#2458=VERTEX_POINT('',#9203);
#2459=VERTEX_POINT('',#9212);
#2460=VERTEX_POINT('',#9214);
#2461=VERTEX_POINT('',#9218);
#2462=VERTEX_POINT('',#9219);
#2463=VERTEX_POINT('',#9224);
#2464=VERTEX_POINT('',#9226);
#2465=VERTEX_POINT('',#9233);
#2466=VERTEX_POINT('',#9234);
#2467=VERTEX_POINT('',#9241);
#2468=VERTEX_POINT('',#9242);
#2469=VERTEX_POINT('',#9249);
#2470=VERTEX_POINT('',#9251);
#2471=VERTEX_POINT('',#9255);
#2472=VERTEX_POINT('',#9256);
#2473=VERTEX_POINT('',#9261);
#2474=VERTEX_POINT('',#9263);
#2475=VERTEX_POINT('',#9272);
#2476=VERTEX_POINT('',#9274);
#2477=VERTEX_POINT('',#9278);
#2478=VERTEX_POINT('',#9283);
#2479=VERTEX_POINT('',#9285);
#2480=VERTEX_POINT('',#9293);
#2481=VERTEX_POINT('',#9302);
#2482=VERTEX_POINT('',#9306);
#2483=VERTEX_POINT('',#9357);
#2484=VERTEX_POINT('',#9363);
#2485=VERTEX_POINT('',#9369);
#2486=VERTEX_POINT('',#9419);
#2487=VERTEX_POINT('',#9421);
#2488=VERTEX_POINT('',#9423);
#2489=VERTEX_POINT('',#9427);
#2490=VERTEX_POINT('',#9430);
#2491=VERTEX_POINT('',#9432);
#2492=VERTEX_POINT('',#9436);
#2493=VERTEX_POINT('',#9438);
#2494=VERTEX_POINT('',#9442);
#2495=VERTEX_POINT('',#9444);
#2496=VERTEX_POINT('',#9448);
#2497=VERTEX_POINT('',#9452);
#2498=VERTEX_POINT('',#9458);
#2499=VERTEX_POINT('',#9460);
#2500=VERTEX_POINT('',#9462);
#2501=VERTEX_POINT('',#9466);
#2502=VERTEX_POINT('',#9469);
#2503=VERTEX_POINT('',#9471);
#2504=VERTEX_POINT('',#9475);
#2505=VERTEX_POINT('',#9477);
#2506=VERTEX_POINT('',#9481);
#2507=VERTEX_POINT('',#9483);
#2508=VERTEX_POINT('',#9487);
#2509=VERTEX_POINT('',#9491);
#2510=VERTEX_POINT('',#9497);
#2511=VERTEX_POINT('',#9499);
#2512=VERTEX_POINT('',#9503);
#2513=VERTEX_POINT('',#9504);
#2514=VERTEX_POINT('',#9506);
#2515=VERTEX_POINT('',#9508);
#2516=VERTEX_POINT('',#9511);
#2517=VERTEX_POINT('',#9514);
#2518=VERTEX_POINT('',#9518);
#2519=VERTEX_POINT('',#9522);
#2520=VERTEX_POINT('',#9526);
#2521=VERTEX_POINT('',#9528);
#2522=VERTEX_POINT('',#9530);
#2523=VERTEX_POINT('',#9534);
#2524=VERTEX_POINT('',#9535);
#2525=VERTEX_POINT('',#9537);
#2526=VERTEX_POINT('',#9539);
#2527=VERTEX_POINT('',#9542);
#2528=VERTEX_POINT('',#9545);
#2529=VERTEX_POINT('',#9549);
#2530=VERTEX_POINT('',#9551);
#2531=VERTEX_POINT('',#9555);
#2532=VERTEX_POINT('',#9559);
#2533=VERTEX_POINT('',#9560);
#2534=VERTEX_POINT('',#9562);
#2535=VERTEX_POINT('',#9566);
#2536=VERTEX_POINT('',#9567);
#2537=VERTEX_POINT('',#9569);
#2538=VERTEX_POINT('',#9573);
#2539=VERTEX_POINT('',#9574);
#2540=VERTEX_POINT('',#9576);
#2541=VERTEX_POINT('',#9583);
#2542=VERTEX_POINT('',#9585);
#2543=VERTEX_POINT('',#9592);
#2544=VERTEX_POINT('',#9593);
#2545=VERTEX_POINT('',#9595);
#2546=VERTEX_POINT('',#9605);
#2547=VERTEX_POINT('',#9607);
#2548=VERTEX_POINT('',#9614);
#2549=VERTEX_POINT('',#9615);
#2550=VERTEX_POINT('',#9620);
#2551=VERTEX_POINT('',#9622);
#2552=VERTEX_POINT('',#9624);
#2553=VERTEX_POINT('',#9628);
#2554=VERTEX_POINT('',#9629);
#2555=VERTEX_POINT('',#9636);
#2556=VERTEX_POINT('',#9637);
#2557=VERTEX_POINT('',#9640);
#2558=VERTEX_POINT('',#9644);
#2559=VERTEX_POINT('',#9645);
#2560=VERTEX_POINT('',#9648);
#2561=VERTEX_POINT('',#9652);
#2562=VERTEX_POINT('',#9653);
#2563=VERTEX_POINT('',#9655);
#2564=VERTEX_POINT('',#9662);
#2565=VERTEX_POINT('',#9664);
#2566=VERTEX_POINT('',#9666);
#2567=VERTEX_POINT('',#9670);
#2568=VERTEX_POINT('',#9671);
#2569=VERTEX_POINT('',#9673);
#2570=VERTEX_POINT('',#9680);
#2571=VERTEX_POINT('',#9681);
#2572=VERTEX_POINT('',#9683);
#2573=VERTEX_POINT('',#9690);
#2574=VERTEX_POINT('',#9691);
#2575=VERTEX_POINT('',#9693);
#2576=VERTEX_POINT('',#9700);
#2577=VERTEX_POINT('',#9701);
#2578=VERTEX_POINT('',#9703);
#2579=VERTEX_POINT('',#9713);
#2580=VERTEX_POINT('',#9714);
#2581=VERTEX_POINT('',#9716);
#2582=VERTEX_POINT('',#9720);
#2583=VERTEX_POINT('',#9721);
#2584=VERTEX_POINT('',#9723);
#2585=VERTEX_POINT('',#9727);
#2586=VERTEX_POINT('',#9729);
#2587=VERTEX_POINT('',#9746);
#2588=VERTEX_POINT('',#9747);
#2589=VERTEX_POINT('',#9749);
#2590=VERTEX_POINT('',#9759);
#2591=VERTEX_POINT('',#9761);
#2592=VERTEX_POINT('',#9778);
#2593=VERTEX_POINT('',#9780);
#2594=VERTEX_POINT('',#9797);
#2595=VERTEX_POINT('',#9799);
#2596=VERTEX_POINT('',#9816);
#2597=VERTEX_POINT('',#9817);
#2598=VERTEX_POINT('',#9819);
#2599=VERTEX_POINT('',#9823);
#2600=VERTEX_POINT('',#9824);
#2601=VERTEX_POINT('',#9826);
#2602=VERTEX_POINT('',#9830);
#2603=VERTEX_POINT('',#9831);
#2604=VERTEX_POINT('',#9833);
#2605=VERTEX_POINT('',#9840);
#2606=VERTEX_POINT('',#9841);
#2607=VERTEX_POINT('',#9843);
#2608=VERTEX_POINT('',#9847);
#2609=VERTEX_POINT('',#9849);
#2610=VERTEX_POINT('',#9872);
#2611=VERTEX_POINT('',#9874);
#2612=VERTEX_POINT('',#9894);
#2613=VERTEX_POINT('',#9896);
#2614=VERTEX_POINT('',#9916);
#2615=VERTEX_POINT('',#9918);
#2616=VERTEX_POINT('',#10000);
#2617=VERTEX_POINT('',#10003);
#2618=VERTEX_POINT('',#10009);
#2619=VERTEX_POINT('',#10011);
#2620=VERTEX_POINT('',#10013);
#2621=VERTEX_POINT('',#10017);
#2622=VERTEX_POINT('',#10020);
#2623=VERTEX_POINT('',#10022);
#2624=VERTEX_POINT('',#10026);
#2625=VERTEX_POINT('',#10028);
#2626=VERTEX_POINT('',#10032);
#2627=VERTEX_POINT('',#10034);
#2628=VERTEX_POINT('',#10038);
#2629=VERTEX_POINT('',#10042);
#2630=VERTEX_POINT('',#10048);
#2631=VERTEX_POINT('',#10051);
#2632=VERTEX_POINT('',#10057);
#2633=VERTEX_POINT('',#10060);
#2634=VERTEX_POINT('',#10066);
#2635=VERTEX_POINT('',#10068);
#2636=VERTEX_POINT('',#10070);
#2637=VERTEX_POINT('',#10074);
#2638=VERTEX_POINT('',#10077);
#2639=VERTEX_POINT('',#10079);
#2640=VERTEX_POINT('',#10083);
#2641=VERTEX_POINT('',#10085);
#2642=VERTEX_POINT('',#10089);
#2643=VERTEX_POINT('',#10091);
#2644=VERTEX_POINT('',#10095);
#2645=VERTEX_POINT('',#10099);
#2646=VERTEX_POINT('',#10105);
#2647=VERTEX_POINT('',#10107);
#2648=VERTEX_POINT('',#10111);
#2649=VERTEX_POINT('',#10112);
#2650=VERTEX_POINT('',#10114);
#2651=VERTEX_POINT('',#10116);
#2652=VERTEX_POINT('',#10119);
#2653=VERTEX_POINT('',#10122);
#2654=VERTEX_POINT('',#10126);
#2655=VERTEX_POINT('',#10130);
#2656=VERTEX_POINT('',#10134);
#2657=VERTEX_POINT('',#10136);
#2658=VERTEX_POINT('',#10138);
#2659=VERTEX_POINT('',#10142);
#2660=VERTEX_POINT('',#10143);
#2661=VERTEX_POINT('',#10145);
#2662=VERTEX_POINT('',#10147);
#2663=VERTEX_POINT('',#10150);
#2664=VERTEX_POINT('',#10153);
#2665=VERTEX_POINT('',#10157);
#2666=VERTEX_POINT('',#10159);
#2667=VERTEX_POINT('',#10163);
#2668=VERTEX_POINT('',#10167);
#2669=VERTEX_POINT('',#10168);
#2670=VERTEX_POINT('',#10170);
#2671=VERTEX_POINT('',#10174);
#2672=VERTEX_POINT('',#10175);
#2673=VERTEX_POINT('',#10177);
#2674=VERTEX_POINT('',#10181);
#2675=VERTEX_POINT('',#10182);
#2676=VERTEX_POINT('',#10184);
#2677=VERTEX_POINT('',#10191);
#2678=VERTEX_POINT('',#10193);
#2679=VERTEX_POINT('',#10200);
#2680=VERTEX_POINT('',#10201);
#2681=VERTEX_POINT('',#10203);
#2682=VERTEX_POINT('',#10213);
#2683=VERTEX_POINT('',#10215);
#2684=VERTEX_POINT('',#10222);
#2685=VERTEX_POINT('',#10223);
#2686=VERTEX_POINT('',#10228);
#2687=VERTEX_POINT('',#10230);
#2688=VERTEX_POINT('',#10232);
#2689=VERTEX_POINT('',#10236);
#2690=VERTEX_POINT('',#10237);
#2691=VERTEX_POINT('',#10244);
#2692=VERTEX_POINT('',#10245);
#2693=VERTEX_POINT('',#10247);
#2694=VERTEX_POINT('',#10252);
#2695=VERTEX_POINT('',#10253);
#2696=VERTEX_POINT('',#10255);
#2697=VERTEX_POINT('',#10260);
#2698=VERTEX_POINT('',#10261);
#2699=VERTEX_POINT('',#10263);
#2700=VERTEX_POINT('',#10270);
#2701=VERTEX_POINT('',#10272);
#2702=VERTEX_POINT('',#10274);
#2703=VERTEX_POINT('',#10278);
#2704=VERTEX_POINT('',#10279);
#2705=VERTEX_POINT('',#10281);
#2706=VERTEX_POINT('',#10288);
#2707=VERTEX_POINT('',#10289);
#2708=VERTEX_POINT('',#10291);
#2709=VERTEX_POINT('',#10298);
#2710=VERTEX_POINT('',#10299);
#2711=VERTEX_POINT('',#10301);
#2712=VERTEX_POINT('',#10308);
#2713=VERTEX_POINT('',#10309);
#2714=VERTEX_POINT('',#10311);
#2715=VERTEX_POINT('',#10321);
#2716=VERTEX_POINT('',#10322);
#2717=VERTEX_POINT('',#10324);
#2718=VERTEX_POINT('',#10328);
#2719=VERTEX_POINT('',#10329);
#2720=VERTEX_POINT('',#10331);
#2721=VERTEX_POINT('',#10335);
#2722=VERTEX_POINT('',#10337);
#2723=VERTEX_POINT('',#10354);
#2724=VERTEX_POINT('',#10355);
#2725=VERTEX_POINT('',#10357);
#2726=VERTEX_POINT('',#10367);
#2727=VERTEX_POINT('',#10369);
#2728=VERTEX_POINT('',#10386);
#2729=VERTEX_POINT('',#10388);
#2730=VERTEX_POINT('',#10405);
#2731=VERTEX_POINT('',#10407);
#2732=VERTEX_POINT('',#10424);
#2733=VERTEX_POINT('',#10425);
#2734=VERTEX_POINT('',#10427);
#2735=VERTEX_POINT('',#10431);
#2736=VERTEX_POINT('',#10432);
#2737=VERTEX_POINT('',#10434);
#2738=VERTEX_POINT('',#10438);
#2739=VERTEX_POINT('',#10439);
#2740=VERTEX_POINT('',#10441);
#2741=VERTEX_POINT('',#10448);
#2742=VERTEX_POINT('',#10449);
#2743=VERTEX_POINT('',#10451);
#2744=VERTEX_POINT('',#10455);
#2745=VERTEX_POINT('',#10457);
#2746=VERTEX_POINT('',#10480);
#2747=VERTEX_POINT('',#10482);
#2748=VERTEX_POINT('',#10502);
#2749=VERTEX_POINT('',#10504);
#2750=VERTEX_POINT('',#10524);
#2751=VERTEX_POINT('',#10526);
#2752=EDGE_CURVE('',#2302,#2302,#1864,.T.);
#2753=EDGE_CURVE('',#2302,#2303,#1204,.T.);
#2754=EDGE_CURVE('',#2303,#2303,#1865,.T.);
#2755=EDGE_CURVE('',#2304,#2305,#1205,.T.);
#2756=EDGE_CURVE('',#2304,#2306,#1206,.T.);
#2757=EDGE_CURVE('',#2307,#2306,#1207,.T.);
#2758=EDGE_CURVE('',#2305,#2307,#1208,.T.);
#2759=EDGE_CURVE('',#2305,#2308,#1209,.T.);
#2760=EDGE_CURVE('',#2309,#2307,#1210,.T.);
#2761=EDGE_CURVE('',#2308,#2309,#1211,.T.);
#2762=EDGE_CURVE('',#2308,#2310,#1212,.T.);
#2763=EDGE_CURVE('',#2311,#2309,#1213,.T.);
#2764=EDGE_CURVE('',#2310,#2311,#1214,.T.);
#2765=EDGE_CURVE('',#2310,#2304,#1215,.T.);
#2766=EDGE_CURVE('',#2306,#2311,#1216,.T.);
#2767=EDGE_CURVE('',#2312,#2312,#1866,.T.);
#2768=EDGE_CURVE('',#2312,#2313,#1867,.T.);
#2769=EDGE_CURVE('',#2313,#2314,#1868,.T.);
#2770=EDGE_CURVE('',#2314,#2313,#1869,.T.);
#2771=EDGE_CURVE('',#2315,#2316,#1217,.T.);
#2772=EDGE_CURVE('',#2317,#2315,#1218,.T.);
#2773=EDGE_CURVE('',#2318,#2317,#1870,.T.);
#2774=EDGE_CURVE('',#2319,#2318,#1219,.T.);
#2775=EDGE_CURVE('',#2320,#2319,#1220,.T.);
#2776=EDGE_CURVE('',#2321,#2320,#1871,.T.);
#2777=EDGE_CURVE('',#2322,#2321,#1221,.T.);
#2778=EDGE_CURVE('',#2323,#2322,#1222,.T.);
#2779=EDGE_CURVE('',#2324,#2323,#1223,.T.);
#2780=EDGE_CURVE('',#2325,#2324,#1224,.T.);
#2781=EDGE_CURVE('',#2326,#2325,#1225,.T.);
#2782=EDGE_CURVE('',#2327,#2326,#1226,.T.);
#2783=EDGE_CURVE('',#2328,#2327,#1227,.T.);
#2784=EDGE_CURVE('',#2329,#2328,#1228,.T.);
#2785=EDGE_CURVE('',#2330,#2329,#1229,.T.);
#2786=EDGE_CURVE('',#2331,#2330,#1230,.T.);
#2787=EDGE_CURVE('',#2332,#2331,#1231,.T.);
#2788=EDGE_CURVE('',#2333,#2332,#1872,.T.);
#2789=EDGE_CURVE('',#2334,#2333,#1232,.T.);
#2790=EDGE_CURVE('',#2335,#2334,#1233,.T.);
#2791=EDGE_CURVE('',#2336,#2335,#1873,.T.);
#2792=EDGE_CURVE('',#2337,#2336,#1234,.T.);
#2793=EDGE_CURVE('',#2338,#2337,#1235,.T.);
#2794=EDGE_CURVE('',#2316,#2338,#1236,.T.);
#2795=EDGE_CURVE('',#2339,#2339,#1874,.T.);
#2796=EDGE_CURVE('',#2314,#2340,#1237,.T.);
#2797=EDGE_CURVE('',#2341,#2340,#1875,.T.);
#2798=EDGE_CURVE('',#2340,#2341,#1876,.T.);
#2799=EDGE_CURVE('',#2342,#2343,#1877,.T.);
#2800=EDGE_CURVE('',#2343,#2339,#1878,.T.);
#2801=EDGE_CURVE('',#2343,#2342,#1879,.T.);
#2802=EDGE_CURVE('',#2342,#2344,#1238,.T.);
#2803=EDGE_CURVE('',#2345,#2344,#1880,.T.);
#2804=EDGE_CURVE('',#2344,#2345,#1881,.T.);
#2805=EDGE_CURVE('',#2346,#2346,#1882,.T.);
#2806=EDGE_CURVE('',#2346,#2341,#1883,.T.);
#2807=EDGE_CURVE('',#2347,#2348,#1884,.T.);
#2808=EDGE_CURVE('',#2349,#2347,#1239,.T.);
#2809=EDGE_CURVE('',#2350,#2349,#1240,.T.);
#2810=EDGE_CURVE('',#2351,#2350,#1241,.T.);
#2811=EDGE_CURVE('',#2352,#2351,#1242,.T.);
#2812=EDGE_CURVE('',#2353,#2352,#1243,.T.);
#2813=EDGE_CURVE('',#2354,#2353,#1885,.T.);
#2814=EDGE_CURVE('',#2355,#2354,#1244,.T.);
#2815=EDGE_CURVE('',#2356,#2355,#1245,.T.);
#2816=EDGE_CURVE('',#2357,#2356,#1886,.T.);
#2817=EDGE_CURVE('',#2358,#2357,#1246,.T.);
#2818=EDGE_CURVE('',#2359,#2358,#1247,.T.);
#2819=EDGE_CURVE('',#2360,#2359,#1248,.T.);
#2820=EDGE_CURVE('',#2361,#2360,#1249,.T.);
#2821=EDGE_CURVE('',#2362,#2361,#1250,.T.);
#2822=EDGE_CURVE('',#2363,#2362,#1251,.T.);
#2823=EDGE_CURVE('',#2364,#2363,#1252,.T.);
#2824=EDGE_CURVE('',#2365,#2364,#1253,.T.);
#2825=EDGE_CURVE('',#2366,#2365,#1254,.T.);
#2826=EDGE_CURVE('',#2367,#2366,#1255,.T.);
#2827=EDGE_CURVE('',#2368,#2367,#1256,.T.);
#2828=EDGE_CURVE('',#2369,#2368,#1887,.T.);
#2829=EDGE_CURVE('',#2370,#2369,#1257,.T.);
#2830=EDGE_CURVE('',#2348,#2370,#1258,.T.);
#2831=EDGE_CURVE('',#2371,#2371,#1888,.T.);
#2832=EDGE_CURVE('',#2345,#2371,#1889,.T.);
#2833=EDGE_CURVE('',#2372,#2372,#1890,.T.);
#2834=EDGE_CURVE('',#2372,#2373,#1891,.T.);
#2835=EDGE_CURVE('',#2373,#2373,#1892,.T.);
#2836=EDGE_CURVE('',#2374,#2375,#1259,.T.);
#2837=EDGE_CURVE('',#2376,#2374,#1260,.T.);
#2838=EDGE_CURVE('',#2377,#2376,#1261,.T.);
#2839=EDGE_CURVE('',#2375,#2377,#1262,.T.);
#2840=EDGE_CURVE('',#2378,#2378,#1893,.T.);
#2841=EDGE_CURVE('',#2379,#2379,#1894,.T.);
#2842=EDGE_CURVE('',#2380,#2380,#1895,.T.);
#2843=EDGE_CURVE('',#2381,#2381,#1896,.T.);
#2844=EDGE_CURVE('',#2382,#2382,#1897,.T.);
#2845=EDGE_CURVE('',#2383,#2383,#1898,.T.);
#2846=EDGE_CURVE('',#2384,#2384,#1899,.T.);
#2847=EDGE_CURVE('',#2385,#2385,#1900,.T.);
#2848=EDGE_CURVE('',#2386,#2386,#1901,.T.);
#2849=EDGE_CURVE('',#2387,#2387,#1902,.T.);
#2850=EDGE_CURVE('',#2388,#2388,#1903,.T.);
#2851=EDGE_CURVE('',#2389,#2389,#1904,.T.);
#2852=EDGE_CURVE('',#2390,#2390,#1905,.T.);
#2853=EDGE_CURVE('',#2391,#2391,#1906,.T.);
#2854=EDGE_CURVE('',#2392,#2392,#1907,.T.);
#2855=EDGE_CURVE('',#2373,#2393,#1263,.T.);
#2856=EDGE_CURVE('',#2393,#2393,#1908,.T.);
#2857=EDGE_CURVE('',#2378,#2394,#1909,.T.);
#2858=EDGE_CURVE('',#2394,#2394,#1910,.T.);
#2859=EDGE_CURVE('',#2394,#2395,#1264,.T.);
#2860=EDGE_CURVE('',#2395,#2395,#1911,.T.);
#2861=EDGE_CURVE('',#2392,#2396,#1912,.T.);
#2862=EDGE_CURVE('',#2396,#2396,#1913,.T.);
#2863=EDGE_CURVE('',#2396,#2397,#1265,.T.);
#2864=EDGE_CURVE('',#2397,#2397,#1914,.T.);
#2865=EDGE_CURVE('',#2379,#2398,#1915,.T.);
#2866=EDGE_CURVE('',#2398,#2398,#1916,.T.);
#2867=EDGE_CURVE('',#2398,#2399,#1266,.T.);
#2868=EDGE_CURVE('',#2399,#2399,#1917,.T.);
#2869=EDGE_CURVE('',#2391,#2400,#1918,.T.);
#2870=EDGE_CURVE('',#2400,#2400,#1919,.T.);
#2871=EDGE_CURVE('',#2400,#2401,#1267,.T.);
#2872=EDGE_CURVE('',#2401,#2401,#1920,.T.);
#2873=EDGE_CURVE('',#2380,#2402,#1921,.T.);
#2874=EDGE_CURVE('',#2402,#2402,#1922,.T.);
#2875=EDGE_CURVE('',#2402,#2403,#1268,.T.);
#2876=EDGE_CURVE('',#2403,#2403,#1923,.T.);
#2877=EDGE_CURVE('',#2390,#2404,#1924,.T.);
#2878=EDGE_CURVE('',#2404,#2404,#1925,.T.);
#2879=EDGE_CURVE('',#2404,#2405,#1269,.T.);
#2880=EDGE_CURVE('',#2405,#2405,#1926,.T.);
#2881=EDGE_CURVE('',#2381,#2406,#1927,.T.);
#2882=EDGE_CURVE('',#2406,#2407,#1928,.T.);
#2883=EDGE_CURVE('',#2407,#2406,#1929,.T.);
#2884=EDGE_CURVE('',#2407,#2408,#1270,.T.);
#2885=EDGE_CURVE('',#2408,#2408,#1930,.T.);
#2886=EDGE_CURVE('',#2389,#2409,#1931,.T.);
#2887=EDGE_CURVE('',#2409,#2409,#1932,.T.);
#2888=EDGE_CURVE('',#2409,#2410,#1271,.T.);
#2889=EDGE_CURVE('',#2410,#2410,#1933,.T.);
#2890=EDGE_CURVE('',#2382,#2411,#1934,.T.);
#2891=EDGE_CURVE('',#2411,#2412,#1935,.T.);
#2892=EDGE_CURVE('',#2412,#2411,#1936,.T.);
#2893=EDGE_CURVE('',#2412,#2413,#1272,.T.);
#2894=EDGE_CURVE('',#2413,#2413,#1937,.T.);
#2895=EDGE_CURVE('',#2388,#2414,#1938,.T.);
#2896=EDGE_CURVE('',#2414,#2414,#1939,.T.);
#2897=EDGE_CURVE('',#2414,#2415,#1273,.T.);
#2898=EDGE_CURVE('',#2415,#2415,#1940,.T.);
#2899=EDGE_CURVE('',#2383,#2416,#1941,.T.);
#2900=EDGE_CURVE('',#2416,#2416,#1942,.T.);
#2901=EDGE_CURVE('',#2416,#2417,#1274,.T.);
#2902=EDGE_CURVE('',#2417,#2417,#1943,.T.);
#2903=EDGE_CURVE('',#2387,#2418,#1944,.T.);
#2904=EDGE_CURVE('',#2418,#2418,#1945,.T.);
#2905=EDGE_CURVE('',#2418,#2419,#1275,.T.);
#2906=EDGE_CURVE('',#2419,#2419,#1946,.T.);
#2907=EDGE_CURVE('',#2384,#2420,#1947,.T.);
#2908=EDGE_CURVE('',#2420,#2420,#1948,.T.);
#2909=EDGE_CURVE('',#2420,#2421,#1276,.T.);
#2910=EDGE_CURVE('',#2421,#2421,#1949,.T.);
#2911=EDGE_CURVE('',#2386,#2422,#1950,.T.);
#2912=EDGE_CURVE('',#2422,#2422,#1951,.T.);
#2913=EDGE_CURVE('',#2422,#2423,#1277,.T.);
#2914=EDGE_CURVE('',#2423,#2423,#1952,.T.);
#2915=EDGE_CURVE('',#2385,#2424,#1953,.T.);
#2916=EDGE_CURVE('',#2424,#2424,#1954,.T.);
#2917=EDGE_CURVE('',#2424,#2425,#1278,.T.);
#2918=EDGE_CURVE('',#2425,#2425,#1955,.T.);
#2919=EDGE_CURVE('',#2326,#2426,#163,.T.);
#2920=EDGE_CURVE('',#2426,#2427,#1279,.T.);
#2921=EDGE_CURVE('',#2327,#2427,#164,.T.);
#2922=EDGE_CURVE('',#2362,#2428,#165,.T.);
#2923=EDGE_CURVE('',#2428,#2429,#1280,.T.);
#2924=EDGE_CURVE('',#2363,#2429,#166,.T.);
#2925=EDGE_CURVE('',#2361,#2430,#167,.T.);
#2926=EDGE_CURVE('',#2430,#2428,#1281,.T.);
#2927=EDGE_CURVE('',#2325,#2431,#168,.T.);
#2928=EDGE_CURVE('',#2431,#2426,#1282,.T.);
#2929=EDGE_CURVE('',#2360,#2432,#169,.T.);
#2930=EDGE_CURVE('',#2432,#2430,#1283,.T.);
#2931=EDGE_CURVE('',#2324,#2433,#170,.T.);
#2932=EDGE_CURVE('',#2433,#2431,#1284,.T.);
#2933=EDGE_CURVE('',#2434,#2435,#1285,.T.);
#2934=EDGE_CURVE('',#2435,#2365,#171,.T.);
#2935=EDGE_CURVE('',#2364,#2434,#172,.T.);
#2936=EDGE_CURVE('',#2359,#2436,#173,.T.);
#2937=EDGE_CURVE('',#2436,#2432,#1286,.T.);
#2938=EDGE_CURVE('',#2437,#2331,#1956,.F.);
#2939=EDGE_CURVE('',#2438,#2437,#1957,.F.);
#2940=EDGE_CURVE('',#2331,#2438,#1958,.F.);
#2941=EDGE_CURVE('',#2439,#2358,#1959,.F.);
#2942=EDGE_CURVE('',#2440,#2439,#1960,.F.);
#2943=EDGE_CURVE('',#2358,#2440,#1961,.F.);
#2944=EDGE_CURVE('',#2437,#2440,#1287,.T.);
#2945=EDGE_CURVE('',#2439,#2438,#1288,.T.);
#2946=EDGE_CURVE('',#2440,#2436,#1289,.T.);
#2947=EDGE_CURVE('',#2441,#2442,#1962,.F.);
#2948=EDGE_CURVE('',#2322,#2441,#1963,.F.);
#2949=EDGE_CURVE('',#2442,#2322,#1964,.F.);
#2950=EDGE_CURVE('',#2441,#2443,#1290,.T.);
#2951=EDGE_CURVE('',#2443,#2323,#174,.T.);
#2952=EDGE_CURVE('',#2444,#2445,#1965,.F.);
#2953=EDGE_CURVE('',#2333,#2444,#1966,.T.);
#2954=EDGE_CURVE('',#2445,#2332,#1967,.T.);
#2955=EDGE_CURVE('',#2367,#2446,#1968,.F.);
#2956=EDGE_CURVE('',#2447,#2367,#1969,.F.);
#2957=EDGE_CURVE('',#2446,#2447,#1970,.F.);
#2958=EDGE_CURVE('',#2448,#2447,#1291,.T.);
#2959=EDGE_CURVE('',#2366,#2448,#175,.T.);
#2960=EDGE_CURVE('',#2442,#2446,#1292,.T.);
#2961=EDGE_CURVE('',#2447,#2441,#1293,.T.);
#2962=EDGE_CURVE('',#2449,#2450,#1971,.F.);
#2963=EDGE_CURVE('',#2357,#2449,#1972,.T.);
#2964=EDGE_CURVE('',#2450,#2356,#1973,.T.);
#2965=EDGE_CURVE('',#2449,#2439,#1294,.T.);
#2966=EDGE_CURVE('',#2451,#2320,#1974,.T.);
#2967=EDGE_CURVE('',#2452,#2451,#1975,.F.);
#2968=EDGE_CURVE('',#2321,#2452,#1976,.T.);
#2969=EDGE_CURVE('',#2453,#2334,#1977,.F.);
#2970=EDGE_CURVE('',#2454,#2453,#1978,.F.);
#2971=EDGE_CURVE('',#2334,#2454,#1979,.F.);
#2972=EDGE_CURVE('',#2455,#2456,#1980,.F.);
#2973=EDGE_CURVE('',#2369,#2455,#1981,.T.);
#2974=EDGE_CURVE('',#2456,#2368,#1982,.T.);
#2975=EDGE_CURVE('',#2457,#2355,#1983,.F.);
#2976=EDGE_CURVE('',#2458,#2457,#1984,.F.);
#2977=EDGE_CURVE('',#2355,#2458,#1985,.F.);
#2978=EDGE_CURVE('',#2453,#2458,#1295,.T.);
#2979=EDGE_CURVE('',#2457,#2454,#1296,.T.);
#2980=EDGE_CURVE('',#2458,#2450,#1297,.T.);
#2981=EDGE_CURVE('',#2459,#2319,#1986,.F.);
#2982=EDGE_CURVE('',#2460,#2459,#1987,.F.);
#2983=EDGE_CURVE('',#2319,#2460,#1988,.F.);
#2984=EDGE_CURVE('',#2461,#2462,#1989,.F.);
#2985=EDGE_CURVE('',#2336,#2461,#1990,.T.);
#2986=EDGE_CURVE('',#2462,#2335,#1991,.T.);
#2987=EDGE_CURVE('',#2463,#2370,#1992,.F.);
#2988=EDGE_CURVE('',#2464,#2463,#1993,.F.);
#2989=EDGE_CURVE('',#2370,#2464,#1994,.F.);
#2990=EDGE_CURVE('',#2459,#2464,#1298,.T.);
#2991=EDGE_CURVE('',#2463,#2460,#1299,.T.);
#2992=EDGE_CURVE('',#2465,#2466,#1995,.F.);
#2993=EDGE_CURVE('',#2354,#2465,#1996,.T.);
#2994=EDGE_CURVE('',#2466,#2353,#1997,.T.);
#2995=EDGE_CURVE('',#2465,#2457,#1300,.T.);
#2996=EDGE_CURVE('',#2467,#2468,#1998,.F.);
#2997=EDGE_CURVE('',#2318,#2467,#1999,.T.);
#2998=EDGE_CURVE('',#2468,#2317,#2000,.T.);
#2999=EDGE_CURVE('',#2467,#2459,#1301,.T.);
#3000=EDGE_CURVE('',#2469,#2337,#2001,.F.);
#3001=EDGE_CURVE('',#2470,#2469,#2002,.F.);
#3002=EDGE_CURVE('',#2337,#2470,#2003,.F.);
#3003=EDGE_CURVE('',#2471,#2472,#2004,.F.);
#3004=EDGE_CURVE('',#2347,#2471,#2005,.T.);
#3005=EDGE_CURVE('',#2472,#2348,#2006,.T.);
#3006=EDGE_CURVE('',#2473,#2352,#2007,.F.);
#3007=EDGE_CURVE('',#2474,#2473,#2008,.F.);
#3008=EDGE_CURVE('',#2352,#2474,#2009,.F.);
#3009=EDGE_CURVE('',#2469,#2474,#1302,.T.);
#3010=EDGE_CURVE('',#2473,#2470,#1303,.T.);
#3011=EDGE_CURVE('',#2474,#2466,#1304,.T.);
#3012=EDGE_CURVE('',#2475,#2315,#2010,.F.);
#3013=EDGE_CURVE('',#2476,#2475,#2011,.F.);
#3014=EDGE_CURVE('',#2315,#2476,#2012,.F.);
#3015=EDGE_CURVE('',#2477,#2338,#2013,.F.);
#3016=EDGE_CURVE('',#2376,#2477,#2014,.F.);
#3017=EDGE_CURVE('',#2338,#2376,#2015,.F.);
#3018=EDGE_CURVE('',#2478,#2349,#2016,.F.);
#3019=EDGE_CURVE('',#2479,#2478,#2017,.F.);
#3020=EDGE_CURVE('',#2349,#2479,#2018,.F.);
#3021=EDGE_CURVE('',#2475,#2479,#1305,.T.);
#3022=EDGE_CURVE('',#2478,#2476,#1306,.T.);
#3023=EDGE_CURVE('',#2377,#2351,#2019,.F.);
#3024=EDGE_CURVE('',#2480,#2377,#2020,.F.);
#3025=EDGE_CURVE('',#2351,#2480,#2021,.F.);
#3026=EDGE_CURVE('',#2477,#2480,#1307,.T.);
#3027=EDGE_CURVE('',#2480,#2473,#1308,.T.);
#3028=EDGE_CURVE('',#2374,#2316,#2022,.F.);
#3029=EDGE_CURVE('',#2481,#2374,#2023,.F.);
#3030=EDGE_CURVE('',#2316,#2481,#2024,.F.);
#3031=EDGE_CURVE('',#2482,#2350,#2025,.F.);
#3032=EDGE_CURVE('',#2375,#2482,#2026,.F.);
#3033=EDGE_CURVE('',#2350,#2375,#2027,.F.);
#3034=EDGE_CURVE('',#2482,#2481,#1309,.T.);
#3035=EDGE_CURVE('',#2479,#2482,#1310,.T.);
#3036=EDGE_CURVE('',#2481,#2475,#1311,.T.);
#3037=EDGE_CURVE('',#2471,#2478,#1312,.T.);
#3038=EDGE_CURVE('',#2470,#2477,#1313,.T.);
#3039=EDGE_CURVE('',#2476,#2468,#1314,.T.);
#3040=EDGE_CURVE('',#2464,#2472,#1315,.T.);
#3041=EDGE_CURVE('',#2468,#2471,#1316,.T.);
#3042=EDGE_CURVE('',#2472,#2467,#1317,.T.);
#3043=EDGE_CURVE('',#2461,#2469,#1318,.T.);
#3044=EDGE_CURVE('',#2466,#2461,#1319,.T.);
#3045=EDGE_CURVE('',#2462,#2465,#1320,.T.);
#3046=EDGE_CURVE('',#2455,#2463,#1321,.T.);
#3047=EDGE_CURVE('',#2454,#2462,#1322,.T.);
#3048=EDGE_CURVE('',#2460,#2451,#1323,.T.);
#3049=EDGE_CURVE('',#2446,#2456,#1324,.T.);
#3050=EDGE_CURVE('',#2451,#2455,#1325,.T.);
#3051=EDGE_CURVE('',#2456,#2452,#1326,.T.);
#3052=EDGE_CURVE('',#2444,#2453,#1327,.T.);
#3053=EDGE_CURVE('',#2452,#2442,#1328,.T.);
#3054=EDGE_CURVE('',#2450,#2444,#1329,.T.);
#3055=EDGE_CURVE('',#2445,#2449,#1330,.T.);
#3056=EDGE_CURVE('',#2438,#2445,#1331,.T.);
#3057=EDGE_CURVE('',#2435,#2448,#1332,.T.);
#3058=EDGE_CURVE('',#2483,#2437,#1333,.T.);
#3059=EDGE_CURVE('',#2330,#2483,#176,.T.);
#3060=EDGE_CURVE('',#2443,#2433,#1334,.T.);
#3061=EDGE_CURVE('',#2484,#2483,#1335,.T.);
#3062=EDGE_CURVE('',#2329,#2484,#177,.T.);
#3063=EDGE_CURVE('',#2429,#2434,#1336,.T.);
#3064=EDGE_CURVE('',#2485,#2484,#1337,.T.);
#3065=EDGE_CURVE('',#2328,#2485,#178,.T.);
#3066=EDGE_CURVE('',#2427,#2485,#1338,.T.);
#3067=EDGE_CURVE('',#2432,#2484,#1339,.T.);
#3068=EDGE_CURVE('',#2483,#2436,#1340,.T.);
#3069=EDGE_CURVE('',#2485,#2430,#1341,.T.);
#3070=EDGE_CURVE('',#2428,#2427,#1342,.T.);
#3071=EDGE_CURVE('',#2426,#2429,#1343,.T.);
#3072=EDGE_CURVE('',#2431,#2434,#1344,.T.);
#3073=EDGE_CURVE('',#2443,#2448,#1345,.T.);
#3074=EDGE_CURVE('',#2433,#2435,#1346,.T.);
#3075=EDGE_CURVE('',#2486,#2486,#2028,.T.);
#3076=EDGE_CURVE('',#2486,#2487,#2029,.T.);
#3077=EDGE_CURVE('',#2488,#2487,#2030,.T.);
#3078=EDGE_CURVE('',#2487,#2488,#2031,.T.);
#3079=EDGE_CURVE('',#2489,#2489,#2032,.T.);
#3080=EDGE_CURVE('',#2488,#2490,#1347,.T.);
#3081=EDGE_CURVE('',#2490,#2491,#2033,.T.);
#3082=EDGE_CURVE('',#2491,#2490,#2034,.T.);
#3083=EDGE_CURVE('',#2489,#2492,#2035,.T.);
#3084=EDGE_CURVE('',#2493,#2492,#2036,.T.);
#3085=EDGE_CURVE('',#2492,#2493,#2037,.T.);
#3086=EDGE_CURVE('',#2493,#2494,#1348,.T.);
#3087=EDGE_CURVE('',#2494,#2495,#2038,.T.);
#3088=EDGE_CURVE('',#2495,#2494,#2039,.T.);
#3089=EDGE_CURVE('',#2496,#2496,#2040,.T.);
#3090=EDGE_CURVE('',#2496,#2491,#2041,.T.);
#3091=EDGE_CURVE('',#2497,#2497,#2042,.T.);
#3092=EDGE_CURVE('',#2497,#2495,#2043,.T.);
#3093=EDGE_CURVE('',#2498,#2498,#2044,.T.);
#3094=EDGE_CURVE('',#2498,#2499,#2045,.T.);
#3095=EDGE_CURVE('',#2499,#2500,#2046,.T.);
#3096=EDGE_CURVE('',#2500,#2499,#2047,.T.);
#3097=EDGE_CURVE('',#2501,#2501,#2048,.T.);
#3098=EDGE_CURVE('',#2500,#2502,#1349,.T.);
#3099=EDGE_CURVE('',#2503,#2502,#2049,.T.);
#3100=EDGE_CURVE('',#2502,#2503,#2050,.T.);
#3101=EDGE_CURVE('',#2501,#2504,#2051,.T.);
#3102=EDGE_CURVE('',#2504,#2505,#2052,.T.);
#3103=EDGE_CURVE('',#2505,#2504,#2053,.T.);
#3104=EDGE_CURVE('',#2505,#2506,#1350,.T.);
#3105=EDGE_CURVE('',#2507,#2506,#2054,.T.);
#3106=EDGE_CURVE('',#2506,#2507,#2055,.T.);
#3107=EDGE_CURVE('',#2508,#2508,#2056,.T.);
#3108=EDGE_CURVE('',#2508,#2503,#2057,.T.);
#3109=EDGE_CURVE('',#2509,#2509,#2058,.T.);
#3110=EDGE_CURVE('',#2509,#2507,#2059,.T.);
#3111=EDGE_CURVE('',#2510,#2510,#2060,.T.);
#3112=EDGE_CURVE('',#2510,#2511,#2061,.T.);
#3113=EDGE_CURVE('',#2511,#2511,#2062,.T.);
#3114=EDGE_CURVE('',#2512,#2513,#1351,.T.);
#3115=EDGE_CURVE('',#2513,#2514,#1352,.T.);
#3116=EDGE_CURVE('',#2514,#2515,#1353,.T.);
#3117=EDGE_CURVE('',#2515,#2512,#1354,.T.);
#3118=EDGE_CURVE('',#2516,#2516,#2063,.T.);
#3119=EDGE_CURVE('',#2510,#2517,#1355,.T.);
#3120=EDGE_CURVE('',#2517,#2517,#2064,.T.);
#3121=EDGE_CURVE('',#2518,#2518,#2065,.T.);
#3122=EDGE_CURVE('',#2518,#2516,#2066,.T.);
#3123=EDGE_CURVE('',#2518,#2519,#1356,.T.);
#3124=EDGE_CURVE('',#2519,#2519,#2067,.T.);
#3125=EDGE_CURVE('',#2520,#2520,#2068,.T.);
#3126=EDGE_CURVE('',#2520,#2521,#2069,.T.);
#3127=EDGE_CURVE('',#2522,#2521,#2070,.T.);
#3128=EDGE_CURVE('',#2521,#2522,#2071,.T.);
#3129=EDGE_CURVE('',#2523,#2524,#1357,.T.);
#3130=EDGE_CURVE('',#2524,#2525,#1358,.T.);
#3131=EDGE_CURVE('',#2525,#2526,#1359,.T.);
#3132=EDGE_CURVE('',#2526,#2523,#1360,.T.);
#3133=EDGE_CURVE('',#2527,#2527,#2072,.T.);
#3134=EDGE_CURVE('',#2522,#2528,#1361,.T.);
#3135=EDGE_CURVE('',#2528,#2528,#2073,.T.);
#3136=EDGE_CURVE('',#2527,#2529,#2074,.T.);
#3137=EDGE_CURVE('',#2530,#2529,#2075,.T.);
#3138=EDGE_CURVE('',#2529,#2530,#2076,.T.);
#3139=EDGE_CURVE('',#2530,#2531,#1362,.T.);
#3140=EDGE_CURVE('',#2531,#2531,#2077,.T.);
#3141=EDGE_CURVE('',#2532,#2533,#2078,.F.);
#3142=EDGE_CURVE('',#2533,#2534,#2079,.F.);
#3143=EDGE_CURVE('',#2534,#2532,#2080,.F.);
#3144=EDGE_CURVE('',#2535,#2536,#2081,.F.);
#3145=EDGE_CURVE('',#2536,#2537,#2082,.F.);
#3146=EDGE_CURVE('',#2537,#2535,#2083,.F.);
#3147=EDGE_CURVE('',#2538,#2539,#2084,.F.);
#3148=EDGE_CURVE('',#2539,#2540,#2085,.F.);
#3149=EDGE_CURVE('',#2540,#2538,#2086,.F.);
#3150=EDGE_CURVE('',#2532,#2540,#1363,.T.);
#3151=EDGE_CURVE('',#2538,#2534,#1364,.T.);
#3152=EDGE_CURVE('',#2541,#2526,#2087,.F.);
#3153=EDGE_CURVE('',#2526,#2542,#2088,.F.);
#3154=EDGE_CURVE('',#2542,#2541,#2089,.F.);
#3155=EDGE_CURVE('',#2533,#2542,#1365,.T.);
#3156=EDGE_CURVE('',#2541,#2532,#1366,.T.);
#3157=EDGE_CURVE('',#2543,#2544,#2090,.F.);
#3158=EDGE_CURVE('',#2544,#2545,#2091,.F.);
#3159=EDGE_CURVE('',#2545,#2543,#2092,.F.);
#3160=EDGE_CURVE('',#2535,#2545,#1367,.T.);
#3161=EDGE_CURVE('',#2543,#2537,#1368,.T.);
#3162=EDGE_CURVE('',#2545,#2538,#1369,.T.);
#3163=EDGE_CURVE('',#2539,#2544,#1370,.T.);
#3164=EDGE_CURVE('',#2546,#2525,#2093,.F.);
#3165=EDGE_CURVE('',#2525,#2547,#2094,.F.);
#3166=EDGE_CURVE('',#2547,#2546,#2095,.F.);
#3167=EDGE_CURVE('',#2537,#2547,#1371,.T.);
#3168=EDGE_CURVE('',#2546,#2536,#1372,.T.);
#3169=EDGE_CURVE('',#2548,#2549,#2096,.F.);
#3170=EDGE_CURVE('',#2549,#2512,#2097,.F.);
#3171=EDGE_CURVE('',#2512,#2548,#2098,.F.);
#3172=EDGE_CURVE('',#2550,#2523,#2099,.F.);
#3173=EDGE_CURVE('',#2523,#2551,#2100,.T.);
#3174=EDGE_CURVE('',#2552,#2551,#2101,.T.);
#3175=EDGE_CURVE('',#2552,#2550,#2102,.T.);
#3176=EDGE_CURVE('',#2553,#2554,#2103,.F.);
#3177=EDGE_CURVE('',#2554,#2513,#2104,.F.);
#3178=EDGE_CURVE('',#2513,#2553,#2105,.F.);
#3179=EDGE_CURVE('',#2553,#2549,#1373,.T.);
#3180=EDGE_CURVE('',#2555,#2556,#2106,.T.);
#3181=EDGE_CURVE('',#2555,#2524,#2107,.T.);
#3182=EDGE_CURVE('',#2524,#2557,#2108,.F.);
#3183=EDGE_CURVE('',#2557,#2556,#2109,.T.);
#3184=EDGE_CURVE('',#2558,#2559,#2110,.T.);
#3185=EDGE_CURVE('',#2558,#2515,#2111,.T.);
#3186=EDGE_CURVE('',#2515,#2560,#2112,.F.);
#3187=EDGE_CURVE('',#2560,#2559,#2113,.T.);
#3188=EDGE_CURVE('',#2561,#2562,#2114,.F.);
#3189=EDGE_CURVE('',#2562,#2563,#2115,.F.);
#3190=EDGE_CURVE('',#2563,#2561,#2116,.F.);
#3191=EDGE_CURVE('',#2561,#2552,#1374,.T.);
#3192=EDGE_CURVE('',#2550,#2563,#1375,.T.);
#3193=EDGE_CURVE('',#2564,#2514,#2117,.F.);
#3194=EDGE_CURVE('',#2514,#2565,#2118,.T.);
#3195=EDGE_CURVE('',#2566,#2565,#2119,.T.);
#3196=EDGE_CURVE('',#2566,#2564,#2120,.T.);
#3197=EDGE_CURVE('',#2567,#2568,#2121,.F.);
#3198=EDGE_CURVE('',#2568,#2569,#2122,.F.);
#3199=EDGE_CURVE('',#2569,#2567,#2123,.F.);
#3200=EDGE_CURVE('',#2556,#2569,#1376,.T.);
#3201=EDGE_CURVE('',#2567,#2557,#1377,.T.);
#3202=EDGE_CURVE('',#2570,#2571,#2124,.F.);
#3203=EDGE_CURVE('',#2571,#2572,#2125,.F.);
#3204=EDGE_CURVE('',#2572,#2570,#2126,.F.);
#3205=EDGE_CURVE('',#2559,#2572,#1378,.T.);
#3206=EDGE_CURVE('',#2570,#2560,#1379,.T.);
#3207=EDGE_CURVE('',#2573,#2574,#2127,.F.);
#3208=EDGE_CURVE('',#2574,#2575,#2128,.F.);
#3209=EDGE_CURVE('',#2575,#2573,#2129,.F.);
#3210=EDGE_CURVE('',#2573,#2561,#1380,.T.);
#3211=EDGE_CURVE('',#2562,#2575,#1381,.T.);
#3212=EDGE_CURVE('',#2576,#2577,#2130,.F.);
#3213=EDGE_CURVE('',#2577,#2578,#2131,.F.);
#3214=EDGE_CURVE('',#2578,#2576,#2132,.F.);
#3215=EDGE_CURVE('',#2564,#2578,#1382,.T.);
#3216=EDGE_CURVE('',#2576,#2566,#1383,.T.);
#3217=EDGE_CURVE('',#2578,#2570,#1384,.T.);
#3218=EDGE_CURVE('',#2571,#2577,#1385,.T.);
#3219=EDGE_CURVE('',#2579,#2580,#2133,.F.);
#3220=EDGE_CURVE('',#2580,#2581,#2134,.F.);
#3221=EDGE_CURVE('',#2581,#2579,#2135,.F.);
#3222=EDGE_CURVE('',#2582,#2583,#2136,.F.);
#3223=EDGE_CURVE('',#2583,#2584,#2137,.F.);
#3224=EDGE_CURVE('',#2584,#2582,#2138,.F.);
#3225=EDGE_CURVE('',#2585,#2573,#1386,.T.);
#3226=EDGE_CURVE('',#2586,#2585,#51,.T.);
#3227=EDGE_CURVE('',#2574,#2586,#1387,.T.);
#3228=EDGE_CURVE('',#2587,#2588,#2139,.F.);
#3229=EDGE_CURVE('',#2588,#2589,#2140,.F.);
#3230=EDGE_CURVE('',#2589,#2587,#2141,.F.);
#3231=EDGE_CURVE('',#2587,#2576,#1388,.T.);
#3232=EDGE_CURVE('',#2577,#2589,#1389,.T.);
#3233=EDGE_CURVE('',#2582,#2588,#1390,.T.);
#3234=EDGE_CURVE('',#2589,#2584,#1391,.T.);
#3235=EDGE_CURVE('',#2590,#2581,#1392,.T.);
#3236=EDGE_CURVE('',#2591,#2590,#52,.T.);
#3237=EDGE_CURVE('',#2579,#2591,#1393,.T.);
#3238=EDGE_CURVE('',#2592,#2582,#1394,.T.);
#3239=EDGE_CURVE('',#2593,#2592,#53,.T.);
#3240=EDGE_CURVE('',#2583,#2593,#1395,.T.);
#3241=EDGE_CURVE('',#2594,#2587,#1396,.T.);
#3242=EDGE_CURVE('',#2595,#2594,#54,.T.);
#3243=EDGE_CURVE('',#2588,#2595,#1397,.T.);
#3244=EDGE_CURVE('',#2596,#2597,#2142,.F.);
#3245=EDGE_CURVE('',#2597,#2598,#2143,.F.);
#3246=EDGE_CURVE('',#2598,#2596,#2144,.F.);
#3247=EDGE_CURVE('',#2599,#2600,#2145,.F.);
#3248=EDGE_CURVE('',#2600,#2601,#2146,.F.);
#3249=EDGE_CURVE('',#2601,#2599,#2147,.F.);
#3250=EDGE_CURVE('',#2602,#2603,#2148,.F.);
#3251=EDGE_CURVE('',#2603,#2604,#2149,.F.);
#3252=EDGE_CURVE('',#2604,#2602,#2150,.F.);
#3253=EDGE_CURVE('',#2602,#2597,#1398,.T.);
#3254=EDGE_CURVE('',#2598,#2604,#1399,.T.);
#3255=EDGE_CURVE('',#2605,#2606,#2151,.F.);
#3256=EDGE_CURVE('',#2606,#2607,#2152,.F.);
#3257=EDGE_CURVE('',#2607,#2605,#2153,.F.);
#3258=EDGE_CURVE('',#2608,#2607,#1400,.T.);
#3259=EDGE_CURVE('',#2609,#2608,#55,.T.);
#3260=EDGE_CURVE('',#2605,#2609,#1401,.T.);
#3261=EDGE_CURVE('',#2607,#2603,#1402,.T.);
#3262=EDGE_CURVE('',#2604,#2606,#1403,.T.);
#3263=EDGE_CURVE('',#2599,#2605,#1404,.T.);
#3264=EDGE_CURVE('',#2606,#2601,#1405,.T.);
#3265=EDGE_CURVE('',#2610,#2602,#1406,.T.);
#3266=EDGE_CURVE('',#2611,#2610,#56,.T.);
#3267=EDGE_CURVE('',#2603,#2611,#1407,.T.);
#3268=EDGE_CURVE('',#2596,#2600,#1408,.T.);
#3269=EDGE_CURVE('',#2601,#2598,#1409,.T.);
#3270=EDGE_CURVE('',#2612,#2599,#1410,.T.);
#3271=EDGE_CURVE('',#2613,#2612,#57,.T.);
#3272=EDGE_CURVE('',#2600,#2613,#1411,.T.);
#3273=EDGE_CURVE('',#2595,#2608,#2154,.T.);
#3274=EDGE_CURVE('',#2609,#2594,#2155,.T.);
#3275=EDGE_CURVE('',#2614,#2596,#1412,.T.);
#3276=EDGE_CURVE('',#2615,#2614,#58,.T.);
#3277=EDGE_CURVE('',#2597,#2615,#1413,.T.);
#3278=EDGE_CURVE('',#2593,#2610,#2156,.T.);
#3279=EDGE_CURVE('',#2611,#2592,#2157,.T.);
#3280=EDGE_CURVE('',#2591,#2612,#2158,.T.);
#3281=EDGE_CURVE('',#2613,#2590,#2159,.T.);
#3282=EDGE_CURVE('',#2586,#2614,#2160,.T.);
#3283=EDGE_CURVE('',#2615,#2585,#2161,.T.);
#3284=EDGE_CURVE('',#2572,#2583,#1414,.T.);
#3285=EDGE_CURVE('',#2584,#2571,#1415,.T.);
#3286=EDGE_CURVE('',#2581,#2574,#1416,.T.);
#3287=EDGE_CURVE('',#2575,#2580,#1417,.T.);
#3288=EDGE_CURVE('',#2569,#2579,#1418,.T.);
#3289=EDGE_CURVE('',#2580,#2568,#1419,.T.);
#3290=EDGE_CURVE('',#2563,#2567,#1420,.T.);
#3291=EDGE_CURVE('',#2568,#2562,#1421,.T.);
#3292=EDGE_CURVE('',#2565,#2554,#1422,.T.);
#3293=EDGE_CURVE('',#2560,#2564,#1423,.T.);
#3294=EDGE_CURVE('',#2548,#2558,#1424,.T.);
#3295=EDGE_CURVE('',#2557,#2550,#1425,.T.);
#3296=EDGE_CURVE('',#2547,#2555,#1426,.T.);
#3297=EDGE_CURVE('',#2544,#2553,#1427,.T.);
#3298=EDGE_CURVE('',#2554,#2543,#1428,.T.);
#3299=EDGE_CURVE('',#2551,#2541,#1429,.T.);
#3300=EDGE_CURVE('',#2540,#2548,#1430,.T.);
#3301=EDGE_CURVE('',#2549,#2539,#1431,.T.);
#3302=EDGE_CURVE('',#2542,#2546,#1432,.T.);
#3303=EDGE_CURVE('',#2536,#2533,#1433,.T.);
#3304=EDGE_CURVE('',#2534,#2535,#1434,.T.);
#3305=EDGE_CURVE('',#2611,#2608,#1435,.T.);
#3306=EDGE_CURVE('',#2592,#2595,#1436,.T.);
#3307=EDGE_CURVE('',#2586,#2590,#1437,.T.);
#3308=EDGE_CURVE('',#2614,#2613,#1438,.T.);
#3309=EDGE_CURVE('',#2616,#2616,#2162,.T.);
#3310=EDGE_CURVE('',#2617,#2617,#2163,.F.);
#3311=EDGE_CURVE('',#2617,#2616,#1439,.T.);
#3312=EDGE_CURVE('',#2618,#2618,#2164,.T.);
#3313=EDGE_CURVE('',#2618,#2619,#2165,.T.);
#3314=EDGE_CURVE('',#2620,#2619,#2166,.T.);
#3315=EDGE_CURVE('',#2619,#2620,#2167,.T.);
#3316=EDGE_CURVE('',#2621,#2621,#2168,.T.);
#3317=EDGE_CURVE('',#2620,#2622,#1440,.T.);
#3318=EDGE_CURVE('',#2622,#2623,#2169,.T.);
#3319=EDGE_CURVE('',#2623,#2622,#2170,.T.);
#3320=EDGE_CURVE('',#2621,#2624,#2171,.T.);
#3321=EDGE_CURVE('',#2625,#2624,#2172,.T.);
#3322=EDGE_CURVE('',#2624,#2625,#2173,.T.);
#3323=EDGE_CURVE('',#2625,#2626,#1441,.T.);
#3324=EDGE_CURVE('',#2626,#2627,#2174,.T.);
#3325=EDGE_CURVE('',#2627,#2626,#2175,.T.);
#3326=EDGE_CURVE('',#2628,#2628,#2176,.T.);
#3327=EDGE_CURVE('',#2628,#2623,#2177,.T.);
#3328=EDGE_CURVE('',#2629,#2629,#2178,.T.);
#3329=EDGE_CURVE('',#2629,#2627,#2179,.T.);
#3330=EDGE_CURVE('',#2630,#2630,#2180,.T.);
#3331=EDGE_CURVE('',#2631,#2631,#2181,.T.);
#3332=EDGE_CURVE('',#2631,#2630,#1442,.T.);
#3333=EDGE_CURVE('',#2632,#2632,#2182,.T.);
#3334=EDGE_CURVE('',#2633,#2633,#2183,.T.);
#3335=EDGE_CURVE('',#2633,#2632,#1443,.T.);
#3336=EDGE_CURVE('',#2634,#2634,#2184,.T.);
#3337=EDGE_CURVE('',#2634,#2635,#2185,.T.);
#3338=EDGE_CURVE('',#2635,#2636,#2186,.T.);
#3339=EDGE_CURVE('',#2636,#2635,#2187,.T.);
#3340=EDGE_CURVE('',#2637,#2637,#2188,.T.);
#3341=EDGE_CURVE('',#2636,#2638,#1444,.T.);
#3342=EDGE_CURVE('',#2639,#2638,#2189,.T.);
#3343=EDGE_CURVE('',#2638,#2639,#2190,.T.);
#3344=EDGE_CURVE('',#2637,#2640,#2191,.T.);
#3345=EDGE_CURVE('',#2640,#2641,#2192,.T.);
#3346=EDGE_CURVE('',#2641,#2640,#2193,.T.);
#3347=EDGE_CURVE('',#2641,#2642,#1445,.T.);
#3348=EDGE_CURVE('',#2643,#2642,#2194,.T.);
#3349=EDGE_CURVE('',#2642,#2643,#2195,.T.);
#3350=EDGE_CURVE('',#2644,#2644,#2196,.T.);
#3351=EDGE_CURVE('',#2644,#2639,#2197,.T.);
#3352=EDGE_CURVE('',#2645,#2645,#2198,.T.);
#3353=EDGE_CURVE('',#2645,#2643,#2199,.T.);
#3354=EDGE_CURVE('',#2646,#2646,#2200,.T.);
#3355=EDGE_CURVE('',#2646,#2647,#2201,.T.);
#3356=EDGE_CURVE('',#2647,#2647,#2202,.T.);
#3357=EDGE_CURVE('',#2648,#2649,#1446,.T.);
#3358=EDGE_CURVE('',#2650,#2648,#1447,.T.);
#3359=EDGE_CURVE('',#2651,#2650,#1448,.T.);
#3360=EDGE_CURVE('',#2649,#2651,#1449,.T.);
#3361=EDGE_CURVE('',#2652,#2652,#2203,.T.);
#3362=EDGE_CURVE('',#2646,#2653,#1450,.T.);
#3363=EDGE_CURVE('',#2653,#2653,#2204,.T.);
#3364=EDGE_CURVE('',#2654,#2654,#2205,.T.);
#3365=EDGE_CURVE('',#2654,#2652,#2206,.T.);
#3366=EDGE_CURVE('',#2654,#2655,#1451,.T.);
#3367=EDGE_CURVE('',#2655,#2655,#2207,.T.);
#3368=EDGE_CURVE('',#2656,#2656,#2208,.T.);
#3369=EDGE_CURVE('',#2656,#2657,#2209,.T.);
#3370=EDGE_CURVE('',#2657,#2658,#2210,.T.);
#3371=EDGE_CURVE('',#2658,#2657,#2211,.T.);
#3372=EDGE_CURVE('',#2659,#2660,#1452,.T.);
#3373=EDGE_CURVE('',#2661,#2659,#1453,.T.);
#3374=EDGE_CURVE('',#2662,#2661,#1454,.T.);
#3375=EDGE_CURVE('',#2660,#2662,#1455,.T.);
#3376=EDGE_CURVE('',#2663,#2663,#2212,.T.);
#3377=EDGE_CURVE('',#2658,#2664,#1456,.T.);
#3378=EDGE_CURVE('',#2664,#2664,#2213,.T.);
#3379=EDGE_CURVE('',#2663,#2665,#2214,.T.);
#3380=EDGE_CURVE('',#2665,#2666,#2215,.T.);
#3381=EDGE_CURVE('',#2666,#2665,#2216,.T.);
#3382=EDGE_CURVE('',#2666,#2667,#1457,.T.);
#3383=EDGE_CURVE('',#2667,#2667,#2217,.T.);
#3384=EDGE_CURVE('',#2668,#2669,#2218,.F.);
#3385=EDGE_CURVE('',#2670,#2668,#2219,.F.);
#3386=EDGE_CURVE('',#2669,#2670,#2220,.F.);
#3387=EDGE_CURVE('',#2671,#2672,#2221,.F.);
#3388=EDGE_CURVE('',#2673,#2671,#2222,.F.);
#3389=EDGE_CURVE('',#2672,#2673,#2223,.F.);
#3390=EDGE_CURVE('',#2674,#2675,#2224,.F.);
#3391=EDGE_CURVE('',#2676,#2674,#2225,.F.);
#3392=EDGE_CURVE('',#2675,#2676,#2226,.F.);
#3393=EDGE_CURVE('',#2674,#2670,#1458,.T.);
#3394=EDGE_CURVE('',#2668,#2676,#1459,.T.);
#3395=EDGE_CURVE('',#2677,#2661,#2227,.F.);
#3396=EDGE_CURVE('',#2678,#2677,#2228,.F.);
#3397=EDGE_CURVE('',#2661,#2678,#2229,.F.);
#3398=EDGE_CURVE('',#2677,#2668,#1460,.T.);
#3399=EDGE_CURVE('',#2669,#2678,#1461,.T.);
#3400=EDGE_CURVE('',#2679,#2680,#2230,.F.);
#3401=EDGE_CURVE('',#2681,#2679,#2231,.F.);
#3402=EDGE_CURVE('',#2680,#2681,#2232,.F.);
#3403=EDGE_CURVE('',#2679,#2673,#1462,.T.);
#3404=EDGE_CURVE('',#2671,#2681,#1463,.T.);
#3405=EDGE_CURVE('',#2675,#2680,#1464,.T.);
#3406=EDGE_CURVE('',#2681,#2674,#1465,.T.);
#3407=EDGE_CURVE('',#2682,#2662,#2233,.F.);
#3408=EDGE_CURVE('',#2683,#2682,#2234,.F.);
#3409=EDGE_CURVE('',#2662,#2683,#2235,.F.);
#3410=EDGE_CURVE('',#2682,#2672,#1466,.T.);
#3411=EDGE_CURVE('',#2673,#2683,#1467,.T.);
#3412=EDGE_CURVE('',#2684,#2685,#2236,.F.);
#3413=EDGE_CURVE('',#2648,#2684,#2237,.F.);
#3414=EDGE_CURVE('',#2685,#2648,#2238,.F.);
#3415=EDGE_CURVE('',#2686,#2659,#2239,.F.);
#3416=EDGE_CURVE('',#2687,#2686,#2240,.T.);
#3417=EDGE_CURVE('',#2687,#2688,#2241,.T.);
#3418=EDGE_CURVE('',#2659,#2688,#2242,.T.);
#3419=EDGE_CURVE('',#2689,#2690,#2243,.F.);
#3420=EDGE_CURVE('',#2649,#2689,#2244,.F.);
#3421=EDGE_CURVE('',#2690,#2649,#2245,.F.);
#3422=EDGE_CURVE('',#2689,#2685,#1468,.T.);
#3423=EDGE_CURVE('',#2691,#2692,#2246,.T.);
#3424=EDGE_CURVE('',#2693,#2692,#2247,.T.);
#3425=EDGE_CURVE('',#2660,#2693,#2248,.F.);
#3426=EDGE_CURVE('',#2691,#2660,#2249,.T.);
#3427=EDGE_CURVE('',#2694,#2695,#2250,.T.);
#3428=EDGE_CURVE('',#2696,#2695,#2251,.T.);
#3429=EDGE_CURVE('',#2650,#2696,#2252,.F.);
#3430=EDGE_CURVE('',#2694,#2650,#2253,.T.);
#3431=EDGE_CURVE('',#2697,#2698,#2254,.F.);
#3432=EDGE_CURVE('',#2699,#2697,#2255,.F.);
#3433=EDGE_CURVE('',#2698,#2699,#2256,.F.);
#3434=EDGE_CURVE('',#2686,#2699,#1469,.T.);
#3435=EDGE_CURVE('',#2697,#2687,#1470,.T.);
#3436=EDGE_CURVE('',#2700,#2651,#2257,.F.);
#3437=EDGE_CURVE('',#2701,#2700,#2258,.T.);
#3438=EDGE_CURVE('',#2701,#2702,#2259,.T.);
#3439=EDGE_CURVE('',#2651,#2702,#2260,.T.);
#3440=EDGE_CURVE('',#2703,#2704,#2261,.F.);
#3441=EDGE_CURVE('',#2705,#2703,#2262,.F.);
#3442=EDGE_CURVE('',#2704,#2705,#2263,.F.);
#3443=EDGE_CURVE('',#2703,#2693,#1471,.T.);
#3444=EDGE_CURVE('',#2692,#2705,#1472,.T.);
#3445=EDGE_CURVE('',#2706,#2707,#2264,.F.);
#3446=EDGE_CURVE('',#2708,#2706,#2265,.F.);
#3447=EDGE_CURVE('',#2707,#2708,#2266,.F.);
#3448=EDGE_CURVE('',#2706,#2696,#1473,.T.);
#3449=EDGE_CURVE('',#2695,#2708,#1474,.T.);
#3450=EDGE_CURVE('',#2709,#2710,#2267,.F.);
#3451=EDGE_CURVE('',#2711,#2709,#2268,.F.);
#3452=EDGE_CURVE('',#2710,#2711,#2269,.F.);
#3453=EDGE_CURVE('',#2698,#2711,#1475,.T.);
#3454=EDGE_CURVE('',#2709,#2697,#1476,.T.);
#3455=EDGE_CURVE('',#2712,#2713,#2270,.F.);
#3456=EDGE_CURVE('',#2714,#2712,#2271,.F.);
#3457=EDGE_CURVE('',#2713,#2714,#2272,.F.);
#3458=EDGE_CURVE('',#2712,#2701,#1477,.T.);
#3459=EDGE_CURVE('',#2700,#2714,#1478,.T.);
#3460=EDGE_CURVE('',#2707,#2713,#1479,.T.);
#3461=EDGE_CURVE('',#2714,#2706,#1480,.T.);
#3462=EDGE_CURVE('',#2715,#2716,#2273,.F.);
#3463=EDGE_CURVE('',#2717,#2715,#2274,.F.);
#3464=EDGE_CURVE('',#2716,#2717,#2275,.F.);
#3465=EDGE_CURVE('',#2718,#2719,#2276,.F.);
#3466=EDGE_CURVE('',#2720,#2718,#2277,.F.);
#3467=EDGE_CURVE('',#2719,#2720,#2278,.F.);
#3468=EDGE_CURVE('',#2721,#2709,#1481,.T.);
#3469=EDGE_CURVE('',#2710,#2722,#1482,.T.);
#3470=EDGE_CURVE('',#2722,#2721,#59,.T.);
#3471=EDGE_CURVE('',#2723,#2724,#2279,.F.);
#3472=EDGE_CURVE('',#2725,#2723,#2280,.F.);
#3473=EDGE_CURVE('',#2724,#2725,#2281,.F.);
#3474=EDGE_CURVE('',#2713,#2725,#1483,.T.);
#3475=EDGE_CURVE('',#2723,#2712,#1484,.T.);
#3476=EDGE_CURVE('',#2725,#2720,#1485,.T.);
#3477=EDGE_CURVE('',#2718,#2724,#1486,.T.);
#3478=EDGE_CURVE('',#2726,#2717,#1487,.T.);
#3479=EDGE_CURVE('',#2715,#2727,#1488,.T.);
#3480=EDGE_CURVE('',#2727,#2726,#60,.T.);
#3481=EDGE_CURVE('',#2728,#2718,#1489,.T.);
#3482=EDGE_CURVE('',#2719,#2729,#1490,.T.);
#3483=EDGE_CURVE('',#2729,#2728,#61,.T.);
#3484=EDGE_CURVE('',#2730,#2723,#1491,.T.);
#3485=EDGE_CURVE('',#2724,#2731,#1492,.T.);
#3486=EDGE_CURVE('',#2731,#2730,#62,.T.);
#3487=EDGE_CURVE('',#2732,#2733,#2282,.F.);
#3488=EDGE_CURVE('',#2734,#2732,#2283,.F.);
#3489=EDGE_CURVE('',#2733,#2734,#2284,.F.);
#3490=EDGE_CURVE('',#2735,#2736,#2285,.F.);
#3491=EDGE_CURVE('',#2737,#2735,#2286,.F.);
#3492=EDGE_CURVE('',#2736,#2737,#2287,.F.);
#3493=EDGE_CURVE('',#2738,#2739,#2288,.F.);
#3494=EDGE_CURVE('',#2740,#2738,#2289,.F.);
#3495=EDGE_CURVE('',#2739,#2740,#2290,.F.);
#3496=EDGE_CURVE('',#2734,#2740,#1493,.T.);
#3497=EDGE_CURVE('',#2738,#2733,#1494,.T.);
#3498=EDGE_CURVE('',#2741,#2742,#2291,.F.);
#3499=EDGE_CURVE('',#2743,#2741,#2292,.F.);
#3500=EDGE_CURVE('',#2742,#2743,#2293,.F.);
#3501=EDGE_CURVE('',#2744,#2743,#1495,.T.);
#3502=EDGE_CURVE('',#2741,#2745,#1496,.T.);
#3503=EDGE_CURVE('',#2745,#2744,#63,.T.);
#3504=EDGE_CURVE('',#2740,#2742,#1497,.T.);
#3505=EDGE_CURVE('',#2743,#2739,#1498,.T.);
#3506=EDGE_CURVE('',#2742,#2737,#1499,.T.);
#3507=EDGE_CURVE('',#2735,#2741,#1500,.T.);
#3508=EDGE_CURVE('',#2746,#2738,#1501,.T.);
#3509=EDGE_CURVE('',#2739,#2747,#1502,.T.);
#3510=EDGE_CURVE('',#2747,#2746,#64,.T.);
#3511=EDGE_CURVE('',#2737,#2734,#1503,.T.);
#3512=EDGE_CURVE('',#2732,#2736,#1504,.T.);
#3513=EDGE_CURVE('',#2748,#2735,#1505,.T.);
#3514=EDGE_CURVE('',#2736,#2749,#1506,.T.);
#3515=EDGE_CURVE('',#2749,#2748,#65,.T.);
#3516=EDGE_CURVE('',#2731,#2744,#2294,.T.);
#3517=EDGE_CURVE('',#2745,#2730,#2295,.T.);
#3518=EDGE_CURVE('',#2750,#2732,#1507,.T.);
#3519=EDGE_CURVE('',#2733,#2751,#1508,.T.);
#3520=EDGE_CURVE('',#2751,#2750,#66,.T.);
#3521=EDGE_CURVE('',#2729,#2746,#2296,.T.);
#3522=EDGE_CURVE('',#2747,#2728,#2297,.T.);
#3523=EDGE_CURVE('',#2727,#2748,#2298,.T.);
#3524=EDGE_CURVE('',#2749,#2726,#2299,.T.);
#3525=EDGE_CURVE('',#2722,#2750,#2300,.T.);
#3526=EDGE_CURVE('',#2751,#2721,#2301,.T.);
#3527=EDGE_CURVE('',#2720,#2707,#1509,.T.);
#3528=EDGE_CURVE('',#2708,#2719,#1510,.T.);
#3529=EDGE_CURVE('',#2711,#2716,#1511,.T.);
#3530=EDGE_CURVE('',#2717,#2710,#1512,.T.);
#3531=EDGE_CURVE('',#2716,#2704,#1513,.T.);
#3532=EDGE_CURVE('',#2705,#2715,#1514,.T.);
#3533=EDGE_CURVE('',#2704,#2698,#1515,.T.);
#3534=EDGE_CURVE('',#2699,#2703,#1516,.T.);
#3535=EDGE_CURVE('',#2702,#2690,#1517,.T.);
#3536=EDGE_CURVE('',#2696,#2700,#1518,.T.);
#3537=EDGE_CURVE('',#2684,#2694,#1519,.T.);
#3538=EDGE_CURVE('',#2693,#2686,#1520,.T.);
#3539=EDGE_CURVE('',#2683,#2691,#1521,.T.);
#3540=EDGE_CURVE('',#2690,#2679,#1522,.T.);
#3541=EDGE_CURVE('',#2680,#2689,#1523,.T.);
#3542=EDGE_CURVE('',#2688,#2677,#1524,.T.);
#3543=EDGE_CURVE('',#2685,#2675,#1525,.T.);
#3544=EDGE_CURVE('',#2676,#2684,#1526,.T.);
#3545=EDGE_CURVE('',#2678,#2682,#1527,.T.);
#3546=EDGE_CURVE('',#2670,#2671,#1528,.T.);
#3547=EDGE_CURVE('',#2672,#2669,#1529,.T.);
#3548=EDGE_CURVE('',#2747,#2744,#1530,.T.);
#3549=EDGE_CURVE('',#2728,#2731,#1531,.T.);
#3550=EDGE_CURVE('',#2750,#2749,#1532,.T.);
#3551=EDGE_CURVE('',#2722,#2726,#1533,.T.);
#3552=ORIENTED_EDGE('',*,*,#2752,.F.);
#3553=ORIENTED_EDGE('',*,*,#2753,.T.);
#3554=ORIENTED_EDGE('',*,*,#2754,.F.);
#3555=ORIENTED_EDGE('',*,*,#2753,.F.);
#3556=ORIENTED_EDGE('',*,*,#2755,.F.);
#3557=ORIENTED_EDGE('',*,*,#2756,.T.);
#3558=ORIENTED_EDGE('',*,*,#2757,.F.);
#3559=ORIENTED_EDGE('',*,*,#2758,.F.);
#3560=ORIENTED_EDGE('',*,*,#2759,.F.);
#3561=ORIENTED_EDGE('',*,*,#2758,.T.);
#3562=ORIENTED_EDGE('',*,*,#2760,.F.);
#3563=ORIENTED_EDGE('',*,*,#2761,.F.);
#3564=ORIENTED_EDGE('',*,*,#2752,.T.);
#3565=ORIENTED_EDGE('',*,*,#2762,.F.);
#3566=ORIENTED_EDGE('',*,*,#2761,.T.);
#3567=ORIENTED_EDGE('',*,*,#2763,.F.);
#3568=ORIENTED_EDGE('',*,*,#2764,.F.);
#3569=ORIENTED_EDGE('',*,*,#2765,.F.);
#3570=ORIENTED_EDGE('',*,*,#2764,.T.);
#3571=ORIENTED_EDGE('',*,*,#2766,.F.);
#3572=ORIENTED_EDGE('',*,*,#2756,.F.);
#3573=ORIENTED_EDGE('',*,*,#2754,.T.);
#3574=ORIENTED_EDGE('',*,*,#2766,.T.);
#3575=ORIENTED_EDGE('',*,*,#2763,.T.);
#3576=ORIENTED_EDGE('',*,*,#2760,.T.);
#3577=ORIENTED_EDGE('',*,*,#2757,.T.);
#3578=ORIENTED_EDGE('',*,*,#2767,.T.);
#3579=ORIENTED_EDGE('',*,*,#2768,.T.);
#3580=ORIENTED_EDGE('',*,*,#2769,.T.);
#3581=ORIENTED_EDGE('',*,*,#2770,.T.);
#3582=ORIENTED_EDGE('',*,*,#2768,.F.);
#3583=ORIENTED_EDGE('',*,*,#2771,.F.);
#3584=ORIENTED_EDGE('',*,*,#2772,.F.);
#3585=ORIENTED_EDGE('',*,*,#2773,.F.);
#3586=ORIENTED_EDGE('',*,*,#2774,.F.);
#3587=ORIENTED_EDGE('',*,*,#2775,.F.);
#3588=ORIENTED_EDGE('',*,*,#2776,.F.);
#3589=ORIENTED_EDGE('',*,*,#2777,.F.);
#3590=ORIENTED_EDGE('',*,*,#2778,.F.);
#3591=ORIENTED_EDGE('',*,*,#2779,.F.);
#3592=ORIENTED_EDGE('',*,*,#2780,.F.);
#3593=ORIENTED_EDGE('',*,*,#2781,.F.);
#3594=ORIENTED_EDGE('',*,*,#2782,.F.);
#3595=ORIENTED_EDGE('',*,*,#2783,.F.);
#3596=ORIENTED_EDGE('',*,*,#2784,.F.);
#3597=ORIENTED_EDGE('',*,*,#2785,.F.);
#3598=ORIENTED_EDGE('',*,*,#2786,.F.);
#3599=ORIENTED_EDGE('',*,*,#2787,.F.);
#3600=ORIENTED_EDGE('',*,*,#2788,.F.);
#3601=ORIENTED_EDGE('',*,*,#2789,.F.);
#3602=ORIENTED_EDGE('',*,*,#2790,.F.);
#3603=ORIENTED_EDGE('',*,*,#2791,.F.);
#3604=ORIENTED_EDGE('',*,*,#2792,.F.);
#3605=ORIENTED_EDGE('',*,*,#2793,.F.);
#3606=ORIENTED_EDGE('',*,*,#2794,.F.);
#3607=ORIENTED_EDGE('',*,*,#2795,.F.);
#3608=ORIENTED_EDGE('',*,*,#2767,.F.);
#3609=ORIENTED_EDGE('',*,*,#2770,.F.);
#3610=ORIENTED_EDGE('',*,*,#2796,.T.);
#3611=ORIENTED_EDGE('',*,*,#2797,.F.);
#3612=ORIENTED_EDGE('',*,*,#2798,.F.);
#3613=ORIENTED_EDGE('',*,*,#2796,.F.);
#3614=ORIENTED_EDGE('',*,*,#2769,.F.);
#3615=ORIENTED_EDGE('',*,*,#2799,.T.);
#3616=ORIENTED_EDGE('',*,*,#2800,.T.);
#3617=ORIENTED_EDGE('',*,*,#2795,.T.);
#3618=ORIENTED_EDGE('',*,*,#2800,.F.);
#3619=ORIENTED_EDGE('',*,*,#2801,.T.);
#3620=ORIENTED_EDGE('',*,*,#2799,.F.);
#3621=ORIENTED_EDGE('',*,*,#2802,.T.);
#3622=ORIENTED_EDGE('',*,*,#2803,.F.);
#3623=ORIENTED_EDGE('',*,*,#2804,.F.);
#3624=ORIENTED_EDGE('',*,*,#2802,.F.);
#3625=ORIENTED_EDGE('',*,*,#2801,.F.);
#3626=ORIENTED_EDGE('',*,*,#2805,.T.);
#3627=ORIENTED_EDGE('',*,*,#2806,.T.);
#3628=ORIENTED_EDGE('',*,*,#2797,.T.);
#3629=ORIENTED_EDGE('',*,*,#2798,.T.);
#3630=ORIENTED_EDGE('',*,*,#2806,.F.);
#3631=ORIENTED_EDGE('',*,*,#2807,.F.);
#3632=ORIENTED_EDGE('',*,*,#2808,.F.);
#3633=ORIENTED_EDGE('',*,*,#2809,.F.);
#3634=ORIENTED_EDGE('',*,*,#2810,.F.);
#3635=ORIENTED_EDGE('',*,*,#2811,.F.);
#3636=ORIENTED_EDGE('',*,*,#2812,.F.);
#3637=ORIENTED_EDGE('',*,*,#2813,.F.);
#3638=ORIENTED_EDGE('',*,*,#2814,.F.);
#3639=ORIENTED_EDGE('',*,*,#2815,.F.);
#3640=ORIENTED_EDGE('',*,*,#2816,.F.);
#3641=ORIENTED_EDGE('',*,*,#2817,.F.);
#3642=ORIENTED_EDGE('',*,*,#2818,.F.);
#3643=ORIENTED_EDGE('',*,*,#2819,.F.);
#3644=ORIENTED_EDGE('',*,*,#2820,.F.);
#3645=ORIENTED_EDGE('',*,*,#2821,.F.);
#3646=ORIENTED_EDGE('',*,*,#2822,.F.);
#3647=ORIENTED_EDGE('',*,*,#2823,.F.);
#3648=ORIENTED_EDGE('',*,*,#2824,.F.);
#3649=ORIENTED_EDGE('',*,*,#2825,.F.);
#3650=ORIENTED_EDGE('',*,*,#2826,.F.);
#3651=ORIENTED_EDGE('',*,*,#2827,.F.);
#3652=ORIENTED_EDGE('',*,*,#2828,.F.);
#3653=ORIENTED_EDGE('',*,*,#2829,.F.);
#3654=ORIENTED_EDGE('',*,*,#2830,.F.);
#3655=ORIENTED_EDGE('',*,*,#2831,.F.);
#3656=ORIENTED_EDGE('',*,*,#2805,.F.);
#3657=ORIENTED_EDGE('',*,*,#2804,.T.);
#3658=ORIENTED_EDGE('',*,*,#2832,.T.);
#3659=ORIENTED_EDGE('',*,*,#2831,.T.);
#3660=ORIENTED_EDGE('',*,*,#2832,.F.);
#3661=ORIENTED_EDGE('',*,*,#2803,.T.);
#3662=ORIENTED_EDGE('',*,*,#2833,.T.);
#3663=ORIENTED_EDGE('',*,*,#2834,.T.);
#3664=ORIENTED_EDGE('',*,*,#2835,.T.);
#3665=ORIENTED_EDGE('',*,*,#2834,.F.);
#3666=ORIENTED_EDGE('',*,*,#2836,.F.);
#3667=ORIENTED_EDGE('',*,*,#2837,.F.);
#3668=ORIENTED_EDGE('',*,*,#2838,.F.);
#3669=ORIENTED_EDGE('',*,*,#2839,.F.);
#3670=ORIENTED_EDGE('',*,*,#2840,.F.);
#3671=ORIENTED_EDGE('',*,*,#2841,.F.);
#3672=ORIENTED_EDGE('',*,*,#2842,.F.);
#3673=ORIENTED_EDGE('',*,*,#2843,.F.);
#3674=ORIENTED_EDGE('',*,*,#2844,.F.);
#3675=ORIENTED_EDGE('',*,*,#2845,.F.);
#3676=ORIENTED_EDGE('',*,*,#2846,.F.);
#3677=ORIENTED_EDGE('',*,*,#2847,.F.);
#3678=ORIENTED_EDGE('',*,*,#2848,.F.);
#3679=ORIENTED_EDGE('',*,*,#2849,.F.);
#3680=ORIENTED_EDGE('',*,*,#2850,.F.);
#3681=ORIENTED_EDGE('',*,*,#2851,.F.);
#3682=ORIENTED_EDGE('',*,*,#2852,.F.);
#3683=ORIENTED_EDGE('',*,*,#2853,.F.);
#3684=ORIENTED_EDGE('',*,*,#2854,.F.);
#3685=ORIENTED_EDGE('',*,*,#2833,.F.);
#3686=ORIENTED_EDGE('',*,*,#2835,.F.);
#3687=ORIENTED_EDGE('',*,*,#2855,.T.);
#3688=ORIENTED_EDGE('',*,*,#2856,.T.);
#3689=ORIENTED_EDGE('',*,*,#2855,.F.);
#3690=ORIENTED_EDGE('',*,*,#2840,.T.);
#3691=ORIENTED_EDGE('',*,*,#2857,.T.);
#3692=ORIENTED_EDGE('',*,*,#2858,.T.);
#3693=ORIENTED_EDGE('',*,*,#2857,.F.);
#3694=ORIENTED_EDGE('',*,*,#2858,.F.);
#3695=ORIENTED_EDGE('',*,*,#2859,.T.);
#3696=ORIENTED_EDGE('',*,*,#2860,.T.);
#3697=ORIENTED_EDGE('',*,*,#2859,.F.);
#3698=ORIENTED_EDGE('',*,*,#2854,.T.);
#3699=ORIENTED_EDGE('',*,*,#2861,.T.);
#3700=ORIENTED_EDGE('',*,*,#2862,.T.);
#3701=ORIENTED_EDGE('',*,*,#2861,.F.);
#3702=ORIENTED_EDGE('',*,*,#2862,.F.);
#3703=ORIENTED_EDGE('',*,*,#2863,.T.);
#3704=ORIENTED_EDGE('',*,*,#2864,.T.);
#3705=ORIENTED_EDGE('',*,*,#2863,.F.);
#3706=ORIENTED_EDGE('',*,*,#2841,.T.);
#3707=ORIENTED_EDGE('',*,*,#2865,.T.);
#3708=ORIENTED_EDGE('',*,*,#2866,.T.);
#3709=ORIENTED_EDGE('',*,*,#2865,.F.);
#3710=ORIENTED_EDGE('',*,*,#2866,.F.);
#3711=ORIENTED_EDGE('',*,*,#2867,.T.);
#3712=ORIENTED_EDGE('',*,*,#2868,.T.);
#3713=ORIENTED_EDGE('',*,*,#2867,.F.);
#3714=ORIENTED_EDGE('',*,*,#2853,.T.);
#3715=ORIENTED_EDGE('',*,*,#2869,.T.);
#3716=ORIENTED_EDGE('',*,*,#2870,.T.);
#3717=ORIENTED_EDGE('',*,*,#2869,.F.);
#3718=ORIENTED_EDGE('',*,*,#2870,.F.);
#3719=ORIENTED_EDGE('',*,*,#2871,.T.);
#3720=ORIENTED_EDGE('',*,*,#2872,.T.);
#3721=ORIENTED_EDGE('',*,*,#2871,.F.);
#3722=ORIENTED_EDGE('',*,*,#2842,.T.);
#3723=ORIENTED_EDGE('',*,*,#2873,.T.);
#3724=ORIENTED_EDGE('',*,*,#2874,.T.);
#3725=ORIENTED_EDGE('',*,*,#2873,.F.);
#3726=ORIENTED_EDGE('',*,*,#2874,.F.);
#3727=ORIENTED_EDGE('',*,*,#2875,.T.);
#3728=ORIENTED_EDGE('',*,*,#2876,.T.);
#3729=ORIENTED_EDGE('',*,*,#2875,.F.);
#3730=ORIENTED_EDGE('',*,*,#2852,.T.);
#3731=ORIENTED_EDGE('',*,*,#2877,.T.);
#3732=ORIENTED_EDGE('',*,*,#2878,.T.);
#3733=ORIENTED_EDGE('',*,*,#2877,.F.);
#3734=ORIENTED_EDGE('',*,*,#2878,.F.);
#3735=ORIENTED_EDGE('',*,*,#2879,.T.);
#3736=ORIENTED_EDGE('',*,*,#2880,.T.);
#3737=ORIENTED_EDGE('',*,*,#2879,.F.);
#3738=ORIENTED_EDGE('',*,*,#2843,.T.);
#3739=ORIENTED_EDGE('',*,*,#2881,.T.);
#3740=ORIENTED_EDGE('',*,*,#2882,.T.);
#3741=ORIENTED_EDGE('',*,*,#2883,.T.);
#3742=ORIENTED_EDGE('',*,*,#2881,.F.);
#3743=ORIENTED_EDGE('',*,*,#2883,.F.);
#3744=ORIENTED_EDGE('',*,*,#2884,.T.);
#3745=ORIENTED_EDGE('',*,*,#2885,.T.);
#3746=ORIENTED_EDGE('',*,*,#2884,.F.);
#3747=ORIENTED_EDGE('',*,*,#2882,.F.);
#3748=ORIENTED_EDGE('',*,*,#2851,.T.);
#3749=ORIENTED_EDGE('',*,*,#2886,.T.);
#3750=ORIENTED_EDGE('',*,*,#2887,.T.);
#3751=ORIENTED_EDGE('',*,*,#2886,.F.);
#3752=ORIENTED_EDGE('',*,*,#2887,.F.);
#3753=ORIENTED_EDGE('',*,*,#2888,.T.);
#3754=ORIENTED_EDGE('',*,*,#2889,.T.);
#3755=ORIENTED_EDGE('',*,*,#2888,.F.);
#3756=ORIENTED_EDGE('',*,*,#2844,.T.);
#3757=ORIENTED_EDGE('',*,*,#2890,.T.);
#3758=ORIENTED_EDGE('',*,*,#2891,.T.);
#3759=ORIENTED_EDGE('',*,*,#2892,.T.);
#3760=ORIENTED_EDGE('',*,*,#2890,.F.);
#3761=ORIENTED_EDGE('',*,*,#2892,.F.);
#3762=ORIENTED_EDGE('',*,*,#2893,.T.);
#3763=ORIENTED_EDGE('',*,*,#2894,.T.);
#3764=ORIENTED_EDGE('',*,*,#2893,.F.);
#3765=ORIENTED_EDGE('',*,*,#2891,.F.);
#3766=ORIENTED_EDGE('',*,*,#2850,.T.);
#3767=ORIENTED_EDGE('',*,*,#2895,.T.);
#3768=ORIENTED_EDGE('',*,*,#2896,.T.);
#3769=ORIENTED_EDGE('',*,*,#2895,.F.);
#3770=ORIENTED_EDGE('',*,*,#2896,.F.);
#3771=ORIENTED_EDGE('',*,*,#2897,.T.);
#3772=ORIENTED_EDGE('',*,*,#2898,.T.);
#3773=ORIENTED_EDGE('',*,*,#2897,.F.);
#3774=ORIENTED_EDGE('',*,*,#2845,.T.);
#3775=ORIENTED_EDGE('',*,*,#2899,.T.);
#3776=ORIENTED_EDGE('',*,*,#2900,.T.);
#3777=ORIENTED_EDGE('',*,*,#2899,.F.);
#3778=ORIENTED_EDGE('',*,*,#2900,.F.);
#3779=ORIENTED_EDGE('',*,*,#2901,.T.);
#3780=ORIENTED_EDGE('',*,*,#2902,.T.);
#3781=ORIENTED_EDGE('',*,*,#2901,.F.);
#3782=ORIENTED_EDGE('',*,*,#2849,.T.);
#3783=ORIENTED_EDGE('',*,*,#2903,.T.);
#3784=ORIENTED_EDGE('',*,*,#2904,.T.);
#3785=ORIENTED_EDGE('',*,*,#2903,.F.);
#3786=ORIENTED_EDGE('',*,*,#2904,.F.);
#3787=ORIENTED_EDGE('',*,*,#2905,.T.);
#3788=ORIENTED_EDGE('',*,*,#2906,.T.);
#3789=ORIENTED_EDGE('',*,*,#2905,.F.);
#3790=ORIENTED_EDGE('',*,*,#2846,.T.);
#3791=ORIENTED_EDGE('',*,*,#2907,.T.);
#3792=ORIENTED_EDGE('',*,*,#2908,.T.);
#3793=ORIENTED_EDGE('',*,*,#2907,.F.);
#3794=ORIENTED_EDGE('',*,*,#2908,.F.);
#3795=ORIENTED_EDGE('',*,*,#2909,.T.);
#3796=ORIENTED_EDGE('',*,*,#2910,.T.);
#3797=ORIENTED_EDGE('',*,*,#2909,.F.);
#3798=ORIENTED_EDGE('',*,*,#2848,.T.);
#3799=ORIENTED_EDGE('',*,*,#2911,.T.);
#3800=ORIENTED_EDGE('',*,*,#2912,.T.);
#3801=ORIENTED_EDGE('',*,*,#2911,.F.);
#3802=ORIENTED_EDGE('',*,*,#2912,.F.);
#3803=ORIENTED_EDGE('',*,*,#2913,.T.);
#3804=ORIENTED_EDGE('',*,*,#2914,.T.);
#3805=ORIENTED_EDGE('',*,*,#2913,.F.);
#3806=ORIENTED_EDGE('',*,*,#2847,.T.);
#3807=ORIENTED_EDGE('',*,*,#2915,.T.);
#3808=ORIENTED_EDGE('',*,*,#2916,.T.);
#3809=ORIENTED_EDGE('',*,*,#2915,.F.);
#3810=ORIENTED_EDGE('',*,*,#2916,.F.);
#3811=ORIENTED_EDGE('',*,*,#2917,.T.);
#3812=ORIENTED_EDGE('',*,*,#2918,.T.);
#3813=ORIENTED_EDGE('',*,*,#2917,.F.);
#3814=ORIENTED_EDGE('',*,*,#2782,.T.);
#3815=ORIENTED_EDGE('',*,*,#2919,.T.);
#3816=ORIENTED_EDGE('',*,*,#2920,.T.);
#3817=ORIENTED_EDGE('',*,*,#2921,.F.);
#3818=ORIENTED_EDGE('',*,*,#2822,.T.);
#3819=ORIENTED_EDGE('',*,*,#2922,.T.);
#3820=ORIENTED_EDGE('',*,*,#2923,.T.);
#3821=ORIENTED_EDGE('',*,*,#2924,.F.);
#3822=ORIENTED_EDGE('',*,*,#2821,.T.);
#3823=ORIENTED_EDGE('',*,*,#2925,.T.);
#3824=ORIENTED_EDGE('',*,*,#2926,.T.);
#3825=ORIENTED_EDGE('',*,*,#2922,.F.);
#3826=ORIENTED_EDGE('',*,*,#2781,.T.);
#3827=ORIENTED_EDGE('',*,*,#2927,.T.);
#3828=ORIENTED_EDGE('',*,*,#2928,.T.);
#3829=ORIENTED_EDGE('',*,*,#2919,.F.);
#3830=ORIENTED_EDGE('',*,*,#2820,.T.);
#3831=ORIENTED_EDGE('',*,*,#2929,.T.);
#3832=ORIENTED_EDGE('',*,*,#2930,.T.);
#3833=ORIENTED_EDGE('',*,*,#2925,.F.);
#3834=ORIENTED_EDGE('',*,*,#2780,.T.);
#3835=ORIENTED_EDGE('',*,*,#2931,.T.);
#3836=ORIENTED_EDGE('',*,*,#2932,.T.);
#3837=ORIENTED_EDGE('',*,*,#2927,.F.);
#3838=ORIENTED_EDGE('',*,*,#2933,.T.);
#3839=ORIENTED_EDGE('',*,*,#2934,.T.);
#3840=ORIENTED_EDGE('',*,*,#2824,.T.);
#3841=ORIENTED_EDGE('',*,*,#2935,.T.);
#3842=ORIENTED_EDGE('',*,*,#2819,.T.);
#3843=ORIENTED_EDGE('',*,*,#2936,.T.);
#3844=ORIENTED_EDGE('',*,*,#2937,.T.);
#3845=ORIENTED_EDGE('',*,*,#2929,.F.);
#3846=ORIENTED_EDGE('',*,*,#2938,.F.);
#3847=ORIENTED_EDGE('',*,*,#2939,.F.);
#3848=ORIENTED_EDGE('',*,*,#2940,.F.);
#3849=ORIENTED_EDGE('',*,*,#2941,.F.);
#3850=ORIENTED_EDGE('',*,*,#2942,.F.);
#3851=ORIENTED_EDGE('',*,*,#2943,.F.);
#3852=ORIENTED_EDGE('',*,*,#2939,.T.);
#3853=ORIENTED_EDGE('',*,*,#2944,.T.);
#3854=ORIENTED_EDGE('',*,*,#2942,.T.);
#3855=ORIENTED_EDGE('',*,*,#2945,.T.);
#3856=ORIENTED_EDGE('',*,*,#2818,.T.);
#3857=ORIENTED_EDGE('',*,*,#2943,.T.);
#3858=ORIENTED_EDGE('',*,*,#2946,.T.);
#3859=ORIENTED_EDGE('',*,*,#2936,.F.);
#3860=ORIENTED_EDGE('',*,*,#2947,.F.);
#3861=ORIENTED_EDGE('',*,*,#2948,.F.);
#3862=ORIENTED_EDGE('',*,*,#2949,.F.);
#3863=ORIENTED_EDGE('',*,*,#2778,.T.);
#3864=ORIENTED_EDGE('',*,*,#2948,.T.);
#3865=ORIENTED_EDGE('',*,*,#2950,.T.);
#3866=ORIENTED_EDGE('',*,*,#2951,.T.);
#3867=ORIENTED_EDGE('',*,*,#2952,.F.);
#3868=ORIENTED_EDGE('',*,*,#2953,.F.);
#3869=ORIENTED_EDGE('',*,*,#2788,.T.);
#3870=ORIENTED_EDGE('',*,*,#2954,.F.);
#3871=ORIENTED_EDGE('',*,*,#2955,.F.);
#3872=ORIENTED_EDGE('',*,*,#2956,.F.);
#3873=ORIENTED_EDGE('',*,*,#2957,.F.);
#3874=ORIENTED_EDGE('',*,*,#2958,.T.);
#3875=ORIENTED_EDGE('',*,*,#2956,.T.);
#3876=ORIENTED_EDGE('',*,*,#2826,.T.);
#3877=ORIENTED_EDGE('',*,*,#2959,.T.);
#3878=ORIENTED_EDGE('',*,*,#2947,.T.);
#3879=ORIENTED_EDGE('',*,*,#2960,.T.);
#3880=ORIENTED_EDGE('',*,*,#2957,.T.);
#3881=ORIENTED_EDGE('',*,*,#2961,.T.);
#3882=ORIENTED_EDGE('',*,*,#2962,.F.);
#3883=ORIENTED_EDGE('',*,*,#2963,.F.);
#3884=ORIENTED_EDGE('',*,*,#2816,.T.);
#3885=ORIENTED_EDGE('',*,*,#2964,.F.);
#3886=ORIENTED_EDGE('',*,*,#2941,.T.);
#3887=ORIENTED_EDGE('',*,*,#2817,.T.);
#3888=ORIENTED_EDGE('',*,*,#2963,.T.);
#3889=ORIENTED_EDGE('',*,*,#2965,.T.);
#3890=ORIENTED_EDGE('',*,*,#2776,.T.);
#3891=ORIENTED_EDGE('',*,*,#2966,.F.);
#3892=ORIENTED_EDGE('',*,*,#2967,.F.);
#3893=ORIENTED_EDGE('',*,*,#2968,.F.);
#3894=ORIENTED_EDGE('',*,*,#2969,.F.);
#3895=ORIENTED_EDGE('',*,*,#2970,.F.);
#3896=ORIENTED_EDGE('',*,*,#2971,.F.);
#3897=ORIENTED_EDGE('',*,*,#2972,.F.);
#3898=ORIENTED_EDGE('',*,*,#2973,.F.);
#3899=ORIENTED_EDGE('',*,*,#2828,.T.);
#3900=ORIENTED_EDGE('',*,*,#2974,.F.);
#3901=ORIENTED_EDGE('',*,*,#2975,.F.);
#3902=ORIENTED_EDGE('',*,*,#2976,.F.);
#3903=ORIENTED_EDGE('',*,*,#2977,.F.);
#3904=ORIENTED_EDGE('',*,*,#2970,.T.);
#3905=ORIENTED_EDGE('',*,*,#2978,.T.);
#3906=ORIENTED_EDGE('',*,*,#2976,.T.);
#3907=ORIENTED_EDGE('',*,*,#2979,.T.);
#3908=ORIENTED_EDGE('',*,*,#2964,.T.);
#3909=ORIENTED_EDGE('',*,*,#2815,.T.);
#3910=ORIENTED_EDGE('',*,*,#2977,.T.);
#3911=ORIENTED_EDGE('',*,*,#2980,.T.);
#3912=ORIENTED_EDGE('',*,*,#2981,.F.);
#3913=ORIENTED_EDGE('',*,*,#2982,.F.);
#3914=ORIENTED_EDGE('',*,*,#2983,.F.);
#3915=ORIENTED_EDGE('',*,*,#2984,.F.);
#3916=ORIENTED_EDGE('',*,*,#2985,.F.);
#3917=ORIENTED_EDGE('',*,*,#2791,.T.);
#3918=ORIENTED_EDGE('',*,*,#2986,.F.);
#3919=ORIENTED_EDGE('',*,*,#2987,.F.);
#3920=ORIENTED_EDGE('',*,*,#2988,.F.);
#3921=ORIENTED_EDGE('',*,*,#2989,.F.);
#3922=ORIENTED_EDGE('',*,*,#2982,.T.);
#3923=ORIENTED_EDGE('',*,*,#2990,.T.);
#3924=ORIENTED_EDGE('',*,*,#2988,.T.);
#3925=ORIENTED_EDGE('',*,*,#2991,.T.);
#3926=ORIENTED_EDGE('',*,*,#2992,.F.);
#3927=ORIENTED_EDGE('',*,*,#2993,.F.);
#3928=ORIENTED_EDGE('',*,*,#2813,.T.);
#3929=ORIENTED_EDGE('',*,*,#2994,.F.);
#3930=ORIENTED_EDGE('',*,*,#2975,.T.);
#3931=ORIENTED_EDGE('',*,*,#2814,.T.);
#3932=ORIENTED_EDGE('',*,*,#2993,.T.);
#3933=ORIENTED_EDGE('',*,*,#2995,.T.);
#3934=ORIENTED_EDGE('',*,*,#2996,.F.);
#3935=ORIENTED_EDGE('',*,*,#2997,.F.);
#3936=ORIENTED_EDGE('',*,*,#2773,.T.);
#3937=ORIENTED_EDGE('',*,*,#2998,.F.);
#3938=ORIENTED_EDGE('',*,*,#2997,.T.);
#3939=ORIENTED_EDGE('',*,*,#2999,.T.);
#3940=ORIENTED_EDGE('',*,*,#2981,.T.);
#3941=ORIENTED_EDGE('',*,*,#2774,.T.);
#3942=ORIENTED_EDGE('',*,*,#3000,.F.);
#3943=ORIENTED_EDGE('',*,*,#3001,.F.);
#3944=ORIENTED_EDGE('',*,*,#3002,.F.);
#3945=ORIENTED_EDGE('',*,*,#3003,.F.);
#3946=ORIENTED_EDGE('',*,*,#3004,.F.);
#3947=ORIENTED_EDGE('',*,*,#2807,.T.);
#3948=ORIENTED_EDGE('',*,*,#3005,.F.);
#3949=ORIENTED_EDGE('',*,*,#3006,.F.);
#3950=ORIENTED_EDGE('',*,*,#3007,.F.);
#3951=ORIENTED_EDGE('',*,*,#3008,.F.);
#3952=ORIENTED_EDGE('',*,*,#3001,.T.);
#3953=ORIENTED_EDGE('',*,*,#3009,.T.);
#3954=ORIENTED_EDGE('',*,*,#3007,.T.);
#3955=ORIENTED_EDGE('',*,*,#3010,.T.);
#3956=ORIENTED_EDGE('',*,*,#2994,.T.);
#3957=ORIENTED_EDGE('',*,*,#2812,.T.);
#3958=ORIENTED_EDGE('',*,*,#3008,.T.);
#3959=ORIENTED_EDGE('',*,*,#3011,.T.);
#3960=ORIENTED_EDGE('',*,*,#3012,.F.);
#3961=ORIENTED_EDGE('',*,*,#3013,.F.);
#3962=ORIENTED_EDGE('',*,*,#3014,.F.);
#3963=ORIENTED_EDGE('',*,*,#3015,.F.);
#3964=ORIENTED_EDGE('',*,*,#3016,.F.);
#3965=ORIENTED_EDGE('',*,*,#3017,.F.);
#3966=ORIENTED_EDGE('',*,*,#3018,.F.);
#3967=ORIENTED_EDGE('',*,*,#3019,.F.);
#3968=ORIENTED_EDGE('',*,*,#3020,.F.);
#3969=ORIENTED_EDGE('',*,*,#3013,.T.);
#3970=ORIENTED_EDGE('',*,*,#3021,.T.);
#3971=ORIENTED_EDGE('',*,*,#3019,.T.);
#3972=ORIENTED_EDGE('',*,*,#3022,.T.);
#3973=ORIENTED_EDGE('',*,*,#3023,.F.);
#3974=ORIENTED_EDGE('',*,*,#3024,.F.);
#3975=ORIENTED_EDGE('',*,*,#3025,.F.);
#3976=ORIENTED_EDGE('',*,*,#3016,.T.);
#3977=ORIENTED_EDGE('',*,*,#3026,.T.);
#3978=ORIENTED_EDGE('',*,*,#3024,.T.);
#3979=ORIENTED_EDGE('',*,*,#2838,.T.);
#3980=ORIENTED_EDGE('',*,*,#3006,.T.);
#3981=ORIENTED_EDGE('',*,*,#2811,.T.);
#3982=ORIENTED_EDGE('',*,*,#3025,.T.);
#3983=ORIENTED_EDGE('',*,*,#3027,.T.);
#3984=ORIENTED_EDGE('',*,*,#3028,.F.);
#3985=ORIENTED_EDGE('',*,*,#3029,.F.);
#3986=ORIENTED_EDGE('',*,*,#3030,.F.);
#3987=ORIENTED_EDGE('',*,*,#3031,.F.);
#3988=ORIENTED_EDGE('',*,*,#3032,.F.);
#3989=ORIENTED_EDGE('',*,*,#3033,.F.);
#3990=ORIENTED_EDGE('',*,*,#3029,.T.);
#3991=ORIENTED_EDGE('',*,*,#2836,.T.);
#3992=ORIENTED_EDGE('',*,*,#3032,.T.);
#3993=ORIENTED_EDGE('',*,*,#3034,.T.);
#3994=ORIENTED_EDGE('',*,*,#3023,.T.);
#3995=ORIENTED_EDGE('',*,*,#2810,.T.);
#3996=ORIENTED_EDGE('',*,*,#3033,.T.);
#3997=ORIENTED_EDGE('',*,*,#2839,.T.);
#3998=ORIENTED_EDGE('',*,*,#3031,.T.);
#3999=ORIENTED_EDGE('',*,*,#2809,.T.);
#4000=ORIENTED_EDGE('',*,*,#3020,.T.);
#4001=ORIENTED_EDGE('',*,*,#3035,.T.);
#4002=ORIENTED_EDGE('',*,*,#3012,.T.);
#4003=ORIENTED_EDGE('',*,*,#2771,.T.);
#4004=ORIENTED_EDGE('',*,*,#3030,.T.);
#4005=ORIENTED_EDGE('',*,*,#3036,.T.);
#4006=ORIENTED_EDGE('',*,*,#3028,.T.);
#4007=ORIENTED_EDGE('',*,*,#2794,.T.);
#4008=ORIENTED_EDGE('',*,*,#3017,.T.);
#4009=ORIENTED_EDGE('',*,*,#2837,.T.);
#4010=ORIENTED_EDGE('',*,*,#3018,.T.);
#4011=ORIENTED_EDGE('',*,*,#2808,.T.);
#4012=ORIENTED_EDGE('',*,*,#3004,.T.);
#4013=ORIENTED_EDGE('',*,*,#3037,.T.);
#4014=ORIENTED_EDGE('',*,*,#3015,.T.);
#4015=ORIENTED_EDGE('',*,*,#2793,.T.);
#4016=ORIENTED_EDGE('',*,*,#3002,.T.);
#4017=ORIENTED_EDGE('',*,*,#3038,.T.);
#4018=ORIENTED_EDGE('',*,*,#2998,.T.);
#4019=ORIENTED_EDGE('',*,*,#2772,.T.);
#4020=ORIENTED_EDGE('',*,*,#3014,.T.);
#4021=ORIENTED_EDGE('',*,*,#3039,.T.);
#4022=ORIENTED_EDGE('',*,*,#2989,.T.);
#4023=ORIENTED_EDGE('',*,*,#3040,.T.);
#4024=ORIENTED_EDGE('',*,*,#3005,.T.);
#4025=ORIENTED_EDGE('',*,*,#2830,.T.);
#4026=ORIENTED_EDGE('',*,*,#2996,.T.);
#4027=ORIENTED_EDGE('',*,*,#3041,.T.);
#4028=ORIENTED_EDGE('',*,*,#3003,.T.);
#4029=ORIENTED_EDGE('',*,*,#3042,.T.);
#4030=ORIENTED_EDGE('',*,*,#3000,.T.);
#4031=ORIENTED_EDGE('',*,*,#2792,.T.);
#4032=ORIENTED_EDGE('',*,*,#2985,.T.);
#4033=ORIENTED_EDGE('',*,*,#3043,.T.);
#4034=ORIENTED_EDGE('',*,*,#2992,.T.);
#4035=ORIENTED_EDGE('',*,*,#3044,.T.);
#4036=ORIENTED_EDGE('',*,*,#2984,.T.);
#4037=ORIENTED_EDGE('',*,*,#3045,.T.);
#4038=ORIENTED_EDGE('',*,*,#2973,.T.);
#4039=ORIENTED_EDGE('',*,*,#3046,.T.);
#4040=ORIENTED_EDGE('',*,*,#2987,.T.);
#4041=ORIENTED_EDGE('',*,*,#2829,.T.);
#4042=ORIENTED_EDGE('',*,*,#2986,.T.);
#4043=ORIENTED_EDGE('',*,*,#2790,.T.);
#4044=ORIENTED_EDGE('',*,*,#2971,.T.);
#4045=ORIENTED_EDGE('',*,*,#3047,.T.);
#4046=ORIENTED_EDGE('',*,*,#2983,.T.);
#4047=ORIENTED_EDGE('',*,*,#3048,.T.);
#4048=ORIENTED_EDGE('',*,*,#2966,.T.);
#4049=ORIENTED_EDGE('',*,*,#2775,.T.);
#4050=ORIENTED_EDGE('',*,*,#2955,.T.);
#4051=ORIENTED_EDGE('',*,*,#3049,.T.);
#4052=ORIENTED_EDGE('',*,*,#2974,.T.);
#4053=ORIENTED_EDGE('',*,*,#2827,.T.);
#4054=ORIENTED_EDGE('',*,*,#2967,.T.);
#4055=ORIENTED_EDGE('',*,*,#3050,.T.);
#4056=ORIENTED_EDGE('',*,*,#2972,.T.);
#4057=ORIENTED_EDGE('',*,*,#3051,.T.);
#4058=ORIENTED_EDGE('',*,*,#2969,.T.);
#4059=ORIENTED_EDGE('',*,*,#2789,.T.);
#4060=ORIENTED_EDGE('',*,*,#2953,.T.);
#4061=ORIENTED_EDGE('',*,*,#3052,.T.);
#4062=ORIENTED_EDGE('',*,*,#2968,.T.);
#4063=ORIENTED_EDGE('',*,*,#3053,.T.);
#4064=ORIENTED_EDGE('',*,*,#2949,.T.);
#4065=ORIENTED_EDGE('',*,*,#2777,.T.);
#4066=ORIENTED_EDGE('',*,*,#2962,.T.);
#4067=ORIENTED_EDGE('',*,*,#3054,.T.);
#4068=ORIENTED_EDGE('',*,*,#2952,.T.);
#4069=ORIENTED_EDGE('',*,*,#3055,.T.);
#4070=ORIENTED_EDGE('',*,*,#2954,.T.);
#4071=ORIENTED_EDGE('',*,*,#2787,.T.);
#4072=ORIENTED_EDGE('',*,*,#2940,.T.);
#4073=ORIENTED_EDGE('',*,*,#3056,.T.);
#4074=ORIENTED_EDGE('',*,*,#3057,.T.);
#4075=ORIENTED_EDGE('',*,*,#2959,.F.);
#4076=ORIENTED_EDGE('',*,*,#2825,.T.);
#4077=ORIENTED_EDGE('',*,*,#2934,.F.);
#4078=ORIENTED_EDGE('',*,*,#3058,.T.);
#4079=ORIENTED_EDGE('',*,*,#2938,.T.);
#4080=ORIENTED_EDGE('',*,*,#2786,.T.);
#4081=ORIENTED_EDGE('',*,*,#3059,.T.);
#4082=ORIENTED_EDGE('',*,*,#2779,.T.);
#4083=ORIENTED_EDGE('',*,*,#2951,.F.);
#4084=ORIENTED_EDGE('',*,*,#3060,.T.);
#4085=ORIENTED_EDGE('',*,*,#2931,.F.);
#4086=ORIENTED_EDGE('',*,*,#3061,.T.);
#4087=ORIENTED_EDGE('',*,*,#3059,.F.);
#4088=ORIENTED_EDGE('',*,*,#2785,.T.);
#4089=ORIENTED_EDGE('',*,*,#3062,.T.);
#4090=ORIENTED_EDGE('',*,*,#3063,.T.);
#4091=ORIENTED_EDGE('',*,*,#2935,.F.);
#4092=ORIENTED_EDGE('',*,*,#2823,.T.);
#4093=ORIENTED_EDGE('',*,*,#2924,.T.);
#4094=ORIENTED_EDGE('',*,*,#3064,.T.);
#4095=ORIENTED_EDGE('',*,*,#3062,.F.);
#4096=ORIENTED_EDGE('',*,*,#2784,.T.);
#4097=ORIENTED_EDGE('',*,*,#3065,.T.);
#4098=ORIENTED_EDGE('',*,*,#3066,.T.);
#4099=ORIENTED_EDGE('',*,*,#3065,.F.);
#4100=ORIENTED_EDGE('',*,*,#2783,.T.);
#4101=ORIENTED_EDGE('',*,*,#2921,.T.);
#4102=ORIENTED_EDGE('',*,*,#3061,.F.);
#4103=ORIENTED_EDGE('',*,*,#3067,.F.);
#4104=ORIENTED_EDGE('',*,*,#2937,.F.);
#4105=ORIENTED_EDGE('',*,*,#3068,.F.);
#4106=ORIENTED_EDGE('',*,*,#3064,.F.);
#4107=ORIENTED_EDGE('',*,*,#3069,.T.);
#4108=ORIENTED_EDGE('',*,*,#2930,.F.);
#4109=ORIENTED_EDGE('',*,*,#3067,.T.);
#4110=ORIENTED_EDGE('',*,*,#3066,.F.);
#4111=ORIENTED_EDGE('',*,*,#3070,.F.);
#4112=ORIENTED_EDGE('',*,*,#2926,.F.);
#4113=ORIENTED_EDGE('',*,*,#3069,.F.);
#4114=ORIENTED_EDGE('',*,*,#2920,.F.);
#4115=ORIENTED_EDGE('',*,*,#3071,.T.);
#4116=ORIENTED_EDGE('',*,*,#2923,.F.);
#4117=ORIENTED_EDGE('',*,*,#3070,.T.);
#4118=ORIENTED_EDGE('',*,*,#2755,.T.);
#4119=ORIENTED_EDGE('',*,*,#2759,.T.);
#4120=ORIENTED_EDGE('',*,*,#2762,.T.);
#4121=ORIENTED_EDGE('',*,*,#2765,.T.);
#4122=ORIENTED_EDGE('',*,*,#2928,.F.);
#4123=ORIENTED_EDGE('',*,*,#3072,.T.);
#4124=ORIENTED_EDGE('',*,*,#3063,.F.);
#4125=ORIENTED_EDGE('',*,*,#3071,.F.);
#4126=ORIENTED_EDGE('',*,*,#2950,.F.);
#4127=ORIENTED_EDGE('',*,*,#2961,.F.);
#4128=ORIENTED_EDGE('',*,*,#2958,.F.);
#4129=ORIENTED_EDGE('',*,*,#3073,.F.);
#4130=ORIENTED_EDGE('',*,*,#2932,.F.);
#4131=ORIENTED_EDGE('',*,*,#3074,.T.);
#4132=ORIENTED_EDGE('',*,*,#2933,.F.);
#4133=ORIENTED_EDGE('',*,*,#3072,.F.);
#4134=ORIENTED_EDGE('',*,*,#3060,.F.);
#4135=ORIENTED_EDGE('',*,*,#3073,.T.);
#4136=ORIENTED_EDGE('',*,*,#3057,.F.);
#4137=ORIENTED_EDGE('',*,*,#3074,.F.);
#4138=ORIENTED_EDGE('',*,*,#2945,.F.);
#4139=ORIENTED_EDGE('',*,*,#2965,.F.);
#4140=ORIENTED_EDGE('',*,*,#3055,.F.);
#4141=ORIENTED_EDGE('',*,*,#3056,.F.);
#4142=ORIENTED_EDGE('',*,*,#2960,.F.);
#4143=ORIENTED_EDGE('',*,*,#3053,.F.);
#4144=ORIENTED_EDGE('',*,*,#3051,.F.);
#4145=ORIENTED_EDGE('',*,*,#3049,.F.);
#4146=ORIENTED_EDGE('',*,*,#2978,.F.);
#4147=ORIENTED_EDGE('',*,*,#3052,.F.);
#4148=ORIENTED_EDGE('',*,*,#3054,.F.);
#4149=ORIENTED_EDGE('',*,*,#2980,.F.);
#4150=ORIENTED_EDGE('',*,*,#2979,.F.);
#4151=ORIENTED_EDGE('',*,*,#2995,.F.);
#4152=ORIENTED_EDGE('',*,*,#3045,.F.);
#4153=ORIENTED_EDGE('',*,*,#3047,.F.);
#4154=ORIENTED_EDGE('',*,*,#2991,.F.);
#4155=ORIENTED_EDGE('',*,*,#3046,.F.);
#4156=ORIENTED_EDGE('',*,*,#3050,.F.);
#4157=ORIENTED_EDGE('',*,*,#3048,.F.);
#4158=ORIENTED_EDGE('',*,*,#2990,.F.);
#4159=ORIENTED_EDGE('',*,*,#2999,.F.);
#4160=ORIENTED_EDGE('',*,*,#3042,.F.);
#4161=ORIENTED_EDGE('',*,*,#3040,.F.);
#4162=ORIENTED_EDGE('',*,*,#3009,.F.);
#4163=ORIENTED_EDGE('',*,*,#3043,.F.);
#4164=ORIENTED_EDGE('',*,*,#3044,.F.);
#4165=ORIENTED_EDGE('',*,*,#3011,.F.);
#4166=ORIENTED_EDGE('',*,*,#3022,.F.);
#4167=ORIENTED_EDGE('',*,*,#3037,.F.);
#4168=ORIENTED_EDGE('',*,*,#3041,.F.);
#4169=ORIENTED_EDGE('',*,*,#3039,.F.);
#4170=ORIENTED_EDGE('',*,*,#3026,.F.);
#4171=ORIENTED_EDGE('',*,*,#3038,.F.);
#4172=ORIENTED_EDGE('',*,*,#3010,.F.);
#4173=ORIENTED_EDGE('',*,*,#3027,.F.);
#4174=ORIENTED_EDGE('',*,*,#3034,.F.);
#4175=ORIENTED_EDGE('',*,*,#3035,.F.);
#4176=ORIENTED_EDGE('',*,*,#3021,.F.);
#4177=ORIENTED_EDGE('',*,*,#3036,.F.);
#4178=ORIENTED_EDGE('',*,*,#3058,.F.);
#4179=ORIENTED_EDGE('',*,*,#3068,.T.);
#4180=ORIENTED_EDGE('',*,*,#2946,.F.);
#4181=ORIENTED_EDGE('',*,*,#2944,.F.);
#4182=ORIENTED_EDGE('',*,*,#2856,.F.);
#4183=ORIENTED_EDGE('',*,*,#2860,.F.);
#4184=ORIENTED_EDGE('',*,*,#2864,.F.);
#4185=ORIENTED_EDGE('',*,*,#2868,.F.);
#4186=ORIENTED_EDGE('',*,*,#2872,.F.);
#4187=ORIENTED_EDGE('',*,*,#2876,.F.);
#4188=ORIENTED_EDGE('',*,*,#2880,.F.);
#4189=ORIENTED_EDGE('',*,*,#2885,.F.);
#4190=ORIENTED_EDGE('',*,*,#2889,.F.);
#4191=ORIENTED_EDGE('',*,*,#2894,.F.);
#4192=ORIENTED_EDGE('',*,*,#2898,.F.);
#4193=ORIENTED_EDGE('',*,*,#2902,.F.);
#4194=ORIENTED_EDGE('',*,*,#2906,.F.);
#4195=ORIENTED_EDGE('',*,*,#2910,.F.);
#4196=ORIENTED_EDGE('',*,*,#2914,.F.);
#4197=ORIENTED_EDGE('',*,*,#2918,.F.);
#4198=ORIENTED_EDGE('',*,*,#3075,.F.);
#4199=ORIENTED_EDGE('',*,*,#3076,.T.);
#4200=ORIENTED_EDGE('',*,*,#3077,.F.);
#4201=ORIENTED_EDGE('',*,*,#3078,.F.);
#4202=ORIENTED_EDGE('',*,*,#3076,.F.);
#4203=ORIENTED_EDGE('',*,*,#3079,.T.);
#4204=ORIENTED_EDGE('',*,*,#3075,.T.);
#4205=ORIENTED_EDGE('',*,*,#3077,.T.);
#4206=ORIENTED_EDGE('',*,*,#3078,.T.);
#4207=ORIENTED_EDGE('',*,*,#3080,.T.);
#4208=ORIENTED_EDGE('',*,*,#3081,.T.);
#4209=ORIENTED_EDGE('',*,*,#3082,.T.);
#4210=ORIENTED_EDGE('',*,*,#3080,.F.);
#4211=ORIENTED_EDGE('',*,*,#3079,.F.);
#4212=ORIENTED_EDGE('',*,*,#3083,.T.);
#4213=ORIENTED_EDGE('',*,*,#3084,.F.);
#4214=ORIENTED_EDGE('',*,*,#3085,.F.);
#4215=ORIENTED_EDGE('',*,*,#3083,.F.);
#4216=ORIENTED_EDGE('',*,*,#3084,.T.);
#4217=ORIENTED_EDGE('',*,*,#3085,.T.);
#4218=ORIENTED_EDGE('',*,*,#3086,.T.);
#4219=ORIENTED_EDGE('',*,*,#3087,.T.);
#4220=ORIENTED_EDGE('',*,*,#3088,.T.);
#4221=ORIENTED_EDGE('',*,*,#3086,.F.);
#4222=ORIENTED_EDGE('',*,*,#3089,.F.);
#4223=ORIENTED_EDGE('',*,*,#3090,.T.);
#4224=ORIENTED_EDGE('',*,*,#3081,.F.);
#4225=ORIENTED_EDGE('',*,*,#3082,.F.);
#4226=ORIENTED_EDGE('',*,*,#3090,.F.);
#4227=ORIENTED_EDGE('',*,*,#3091,.T.);
#4228=ORIENTED_EDGE('',*,*,#3089,.T.);
#4229=ORIENTED_EDGE('',*,*,#3091,.F.);
#4230=ORIENTED_EDGE('',*,*,#3092,.T.);
#4231=ORIENTED_EDGE('',*,*,#3087,.F.);
#4232=ORIENTED_EDGE('',*,*,#3088,.F.);
#4233=ORIENTED_EDGE('',*,*,#3092,.F.);
#4234=ORIENTED_EDGE('',*,*,#3093,.T.);
#4235=ORIENTED_EDGE('',*,*,#3094,.T.);
#4236=ORIENTED_EDGE('',*,*,#3095,.T.);
#4237=ORIENTED_EDGE('',*,*,#3096,.T.);
#4238=ORIENTED_EDGE('',*,*,#3094,.F.);
#4239=ORIENTED_EDGE('',*,*,#3097,.F.);
#4240=ORIENTED_EDGE('',*,*,#3093,.F.);
#4241=ORIENTED_EDGE('',*,*,#3096,.F.);
#4242=ORIENTED_EDGE('',*,*,#3098,.T.);
#4243=ORIENTED_EDGE('',*,*,#3099,.F.);
#4244=ORIENTED_EDGE('',*,*,#3100,.F.);
#4245=ORIENTED_EDGE('',*,*,#3098,.F.);
#4246=ORIENTED_EDGE('',*,*,#3095,.F.);
#4247=ORIENTED_EDGE('',*,*,#3097,.T.);
#4248=ORIENTED_EDGE('',*,*,#3101,.T.);
#4249=ORIENTED_EDGE('',*,*,#3102,.T.);
#4250=ORIENTED_EDGE('',*,*,#3103,.T.);
#4251=ORIENTED_EDGE('',*,*,#3101,.F.);
#4252=ORIENTED_EDGE('',*,*,#3103,.F.);
#4253=ORIENTED_EDGE('',*,*,#3104,.T.);
#4254=ORIENTED_EDGE('',*,*,#3105,.F.);
#4255=ORIENTED_EDGE('',*,*,#3106,.F.);
#4256=ORIENTED_EDGE('',*,*,#3104,.F.);
#4257=ORIENTED_EDGE('',*,*,#3102,.F.);
#4258=ORIENTED_EDGE('',*,*,#3107,.T.);
#4259=ORIENTED_EDGE('',*,*,#3108,.T.);
#4260=ORIENTED_EDGE('',*,*,#3099,.T.);
#4261=ORIENTED_EDGE('',*,*,#3100,.T.);
#4262=ORIENTED_EDGE('',*,*,#3108,.F.);
#4263=ORIENTED_EDGE('',*,*,#3109,.F.);
#4264=ORIENTED_EDGE('',*,*,#3107,.F.);
#4265=ORIENTED_EDGE('',*,*,#3109,.T.);
#4266=ORIENTED_EDGE('',*,*,#3110,.T.);
#4267=ORIENTED_EDGE('',*,*,#3105,.T.);
#4268=ORIENTED_EDGE('',*,*,#3106,.T.);
#4269=ORIENTED_EDGE('',*,*,#3110,.F.);
#4270=ORIENTED_EDGE('',*,*,#3111,.F.);
#4271=ORIENTED_EDGE('',*,*,#3112,.T.);
#4272=ORIENTED_EDGE('',*,*,#3113,.F.);
#4273=ORIENTED_EDGE('',*,*,#3112,.F.);
#4274=ORIENTED_EDGE('',*,*,#3114,.T.);
#4275=ORIENTED_EDGE('',*,*,#3115,.T.);
#4276=ORIENTED_EDGE('',*,*,#3116,.T.);
#4277=ORIENTED_EDGE('',*,*,#3117,.T.);
#4278=ORIENTED_EDGE('',*,*,#3118,.T.);
#4279=ORIENTED_EDGE('',*,*,#3113,.T.);
#4280=ORIENTED_EDGE('',*,*,#3111,.T.);
#4281=ORIENTED_EDGE('',*,*,#3119,.T.);
#4282=ORIENTED_EDGE('',*,*,#3120,.F.);
#4283=ORIENTED_EDGE('',*,*,#3119,.F.);
#4284=ORIENTED_EDGE('',*,*,#3121,.F.);
#4285=ORIENTED_EDGE('',*,*,#3122,.T.);
#4286=ORIENTED_EDGE('',*,*,#3118,.F.);
#4287=ORIENTED_EDGE('',*,*,#3122,.F.);
#4288=ORIENTED_EDGE('',*,*,#3121,.T.);
#4289=ORIENTED_EDGE('',*,*,#3123,.T.);
#4290=ORIENTED_EDGE('',*,*,#3124,.F.);
#4291=ORIENTED_EDGE('',*,*,#3123,.F.);
#4292=ORIENTED_EDGE('',*,*,#3125,.F.);
#4293=ORIENTED_EDGE('',*,*,#3126,.T.);
#4294=ORIENTED_EDGE('',*,*,#3127,.F.);
#4295=ORIENTED_EDGE('',*,*,#3128,.F.);
#4296=ORIENTED_EDGE('',*,*,#3126,.F.);
#4297=ORIENTED_EDGE('',*,*,#3129,.T.);
#4298=ORIENTED_EDGE('',*,*,#3130,.T.);
#4299=ORIENTED_EDGE('',*,*,#3131,.T.);
#4300=ORIENTED_EDGE('',*,*,#3132,.T.);
#4301=ORIENTED_EDGE('',*,*,#3133,.T.);
#4302=ORIENTED_EDGE('',*,*,#3125,.T.);
#4303=ORIENTED_EDGE('',*,*,#3127,.T.);
#4304=ORIENTED_EDGE('',*,*,#3128,.T.);
#4305=ORIENTED_EDGE('',*,*,#3134,.T.);
#4306=ORIENTED_EDGE('',*,*,#3135,.T.);
#4307=ORIENTED_EDGE('',*,*,#3134,.F.);
#4308=ORIENTED_EDGE('',*,*,#3133,.F.);
#4309=ORIENTED_EDGE('',*,*,#3136,.T.);
#4310=ORIENTED_EDGE('',*,*,#3137,.F.);
#4311=ORIENTED_EDGE('',*,*,#3138,.F.);
#4312=ORIENTED_EDGE('',*,*,#3136,.F.);
#4313=ORIENTED_EDGE('',*,*,#3137,.T.);
#4314=ORIENTED_EDGE('',*,*,#3138,.T.);
#4315=ORIENTED_EDGE('',*,*,#3139,.T.);
#4316=ORIENTED_EDGE('',*,*,#3140,.T.);
#4317=ORIENTED_EDGE('',*,*,#3139,.F.);
#4318=ORIENTED_EDGE('',*,*,#3141,.T.);
#4319=ORIENTED_EDGE('',*,*,#3142,.T.);
#4320=ORIENTED_EDGE('',*,*,#3143,.T.);
#4321=ORIENTED_EDGE('',*,*,#3144,.T.);
#4322=ORIENTED_EDGE('',*,*,#3145,.T.);
#4323=ORIENTED_EDGE('',*,*,#3146,.T.);
#4324=ORIENTED_EDGE('',*,*,#3147,.T.);
#4325=ORIENTED_EDGE('',*,*,#3148,.T.);
#4326=ORIENTED_EDGE('',*,*,#3149,.T.);
#4327=ORIENTED_EDGE('',*,*,#3149,.F.);
#4328=ORIENTED_EDGE('',*,*,#3150,.F.);
#4329=ORIENTED_EDGE('',*,*,#3143,.F.);
#4330=ORIENTED_EDGE('',*,*,#3151,.F.);
#4331=ORIENTED_EDGE('',*,*,#3152,.T.);
#4332=ORIENTED_EDGE('',*,*,#3153,.T.);
#4333=ORIENTED_EDGE('',*,*,#3154,.T.);
#4334=ORIENTED_EDGE('',*,*,#3154,.F.);
#4335=ORIENTED_EDGE('',*,*,#3155,.F.);
#4336=ORIENTED_EDGE('',*,*,#3141,.F.);
#4337=ORIENTED_EDGE('',*,*,#3156,.F.);
#4338=ORIENTED_EDGE('',*,*,#3157,.T.);
#4339=ORIENTED_EDGE('',*,*,#3158,.T.);
#4340=ORIENTED_EDGE('',*,*,#3159,.T.);
#4341=ORIENTED_EDGE('',*,*,#3159,.F.);
#4342=ORIENTED_EDGE('',*,*,#3160,.F.);
#4343=ORIENTED_EDGE('',*,*,#3146,.F.);
#4344=ORIENTED_EDGE('',*,*,#3161,.F.);
#4345=ORIENTED_EDGE('',*,*,#3147,.F.);
#4346=ORIENTED_EDGE('',*,*,#3162,.F.);
#4347=ORIENTED_EDGE('',*,*,#3158,.F.);
#4348=ORIENTED_EDGE('',*,*,#3163,.F.);
#4349=ORIENTED_EDGE('',*,*,#3164,.T.);
#4350=ORIENTED_EDGE('',*,*,#3165,.T.);
#4351=ORIENTED_EDGE('',*,*,#3166,.T.);
#4352=ORIENTED_EDGE('',*,*,#3166,.F.);
#4353=ORIENTED_EDGE('',*,*,#3167,.F.);
#4354=ORIENTED_EDGE('',*,*,#3145,.F.);
#4355=ORIENTED_EDGE('',*,*,#3168,.F.);
#4356=ORIENTED_EDGE('',*,*,#3169,.T.);
#4357=ORIENTED_EDGE('',*,*,#3170,.T.);
#4358=ORIENTED_EDGE('',*,*,#3171,.T.);
#4359=ORIENTED_EDGE('',*,*,#3172,.T.);
#4360=ORIENTED_EDGE('',*,*,#3173,.T.);
#4361=ORIENTED_EDGE('',*,*,#3174,.F.);
#4362=ORIENTED_EDGE('',*,*,#3175,.T.);
#4363=ORIENTED_EDGE('',*,*,#3176,.T.);
#4364=ORIENTED_EDGE('',*,*,#3177,.T.);
#4365=ORIENTED_EDGE('',*,*,#3178,.T.);
#4366=ORIENTED_EDGE('',*,*,#3178,.F.);
#4367=ORIENTED_EDGE('',*,*,#3114,.F.);
#4368=ORIENTED_EDGE('',*,*,#3170,.F.);
#4369=ORIENTED_EDGE('',*,*,#3179,.F.);
#4370=ORIENTED_EDGE('',*,*,#3180,.F.);
#4371=ORIENTED_EDGE('',*,*,#3181,.T.);
#4372=ORIENTED_EDGE('',*,*,#3182,.T.);
#4373=ORIENTED_EDGE('',*,*,#3183,.T.);
#4374=ORIENTED_EDGE('',*,*,#3184,.F.);
#4375=ORIENTED_EDGE('',*,*,#3185,.T.);
#4376=ORIENTED_EDGE('',*,*,#3186,.T.);
#4377=ORIENTED_EDGE('',*,*,#3187,.T.);
#4378=ORIENTED_EDGE('',*,*,#3188,.T.);
#4379=ORIENTED_EDGE('',*,*,#3189,.T.);
#4380=ORIENTED_EDGE('',*,*,#3190,.T.);
#4381=ORIENTED_EDGE('',*,*,#3175,.F.);
#4382=ORIENTED_EDGE('',*,*,#3191,.F.);
#4383=ORIENTED_EDGE('',*,*,#3190,.F.);
#4384=ORIENTED_EDGE('',*,*,#3192,.F.);
#4385=ORIENTED_EDGE('',*,*,#3193,.T.);
#4386=ORIENTED_EDGE('',*,*,#3194,.T.);
#4387=ORIENTED_EDGE('',*,*,#3195,.F.);
#4388=ORIENTED_EDGE('',*,*,#3196,.T.);
#4389=ORIENTED_EDGE('',*,*,#3197,.T.);
#4390=ORIENTED_EDGE('',*,*,#3198,.T.);
#4391=ORIENTED_EDGE('',*,*,#3199,.T.);
#4392=ORIENTED_EDGE('',*,*,#3199,.F.);
#4393=ORIENTED_EDGE('',*,*,#3200,.F.);
#4394=ORIENTED_EDGE('',*,*,#3183,.F.);
#4395=ORIENTED_EDGE('',*,*,#3201,.F.);
#4396=ORIENTED_EDGE('',*,*,#3202,.T.);
#4397=ORIENTED_EDGE('',*,*,#3203,.T.);
#4398=ORIENTED_EDGE('',*,*,#3204,.T.);
#4399=ORIENTED_EDGE('',*,*,#3204,.F.);
#4400=ORIENTED_EDGE('',*,*,#3205,.F.);
#4401=ORIENTED_EDGE('',*,*,#3187,.F.);
#4402=ORIENTED_EDGE('',*,*,#3206,.F.);
#4403=ORIENTED_EDGE('',*,*,#3207,.T.);
#4404=ORIENTED_EDGE('',*,*,#3208,.T.);
#4405=ORIENTED_EDGE('',*,*,#3209,.T.);
#4406=ORIENTED_EDGE('',*,*,#3188,.F.);
#4407=ORIENTED_EDGE('',*,*,#3210,.F.);
#4408=ORIENTED_EDGE('',*,*,#3209,.F.);
#4409=ORIENTED_EDGE('',*,*,#3211,.F.);
#4410=ORIENTED_EDGE('',*,*,#3212,.T.);
#4411=ORIENTED_EDGE('',*,*,#3213,.T.);
#4412=ORIENTED_EDGE('',*,*,#3214,.T.);
#4413=ORIENTED_EDGE('',*,*,#3214,.F.);
#4414=ORIENTED_EDGE('',*,*,#3215,.F.);
#4415=ORIENTED_EDGE('',*,*,#3196,.F.);
#4416=ORIENTED_EDGE('',*,*,#3216,.F.);
#4417=ORIENTED_EDGE('',*,*,#3202,.F.);
#4418=ORIENTED_EDGE('',*,*,#3217,.F.);
#4419=ORIENTED_EDGE('',*,*,#3213,.F.);
#4420=ORIENTED_EDGE('',*,*,#3218,.F.);
#4421=ORIENTED_EDGE('',*,*,#3219,.T.);
#4422=ORIENTED_EDGE('',*,*,#3220,.T.);
#4423=ORIENTED_EDGE('',*,*,#3221,.T.);
#4424=ORIENTED_EDGE('',*,*,#3222,.T.);
#4425=ORIENTED_EDGE('',*,*,#3223,.T.);
#4426=ORIENTED_EDGE('',*,*,#3224,.T.);
#4427=ORIENTED_EDGE('',*,*,#3225,.F.);
#4428=ORIENTED_EDGE('',*,*,#3226,.F.);
#4429=ORIENTED_EDGE('',*,*,#3227,.F.);
#4430=ORIENTED_EDGE('',*,*,#3207,.F.);
#4431=ORIENTED_EDGE('',*,*,#3228,.T.);
#4432=ORIENTED_EDGE('',*,*,#3229,.T.);
#4433=ORIENTED_EDGE('',*,*,#3230,.T.);
#4434=ORIENTED_EDGE('',*,*,#3212,.F.);
#4435=ORIENTED_EDGE('',*,*,#3231,.F.);
#4436=ORIENTED_EDGE('',*,*,#3230,.F.);
#4437=ORIENTED_EDGE('',*,*,#3232,.F.);
#4438=ORIENTED_EDGE('',*,*,#3229,.F.);
#4439=ORIENTED_EDGE('',*,*,#3233,.F.);
#4440=ORIENTED_EDGE('',*,*,#3224,.F.);
#4441=ORIENTED_EDGE('',*,*,#3234,.F.);
#4442=ORIENTED_EDGE('',*,*,#3235,.F.);
#4443=ORIENTED_EDGE('',*,*,#3236,.F.);
#4444=ORIENTED_EDGE('',*,*,#3237,.F.);
#4445=ORIENTED_EDGE('',*,*,#3221,.F.);
#4446=ORIENTED_EDGE('',*,*,#3238,.F.);
#4447=ORIENTED_EDGE('',*,*,#3239,.F.);
#4448=ORIENTED_EDGE('',*,*,#3240,.F.);
#4449=ORIENTED_EDGE('',*,*,#3222,.F.);
#4450=ORIENTED_EDGE('',*,*,#3241,.F.);
#4451=ORIENTED_EDGE('',*,*,#3242,.F.);
#4452=ORIENTED_EDGE('',*,*,#3243,.F.);
#4453=ORIENTED_EDGE('',*,*,#3228,.F.);
#4454=ORIENTED_EDGE('',*,*,#3244,.T.);
#4455=ORIENTED_EDGE('',*,*,#3245,.T.);
#4456=ORIENTED_EDGE('',*,*,#3246,.T.);
#4457=ORIENTED_EDGE('',*,*,#3247,.T.);
#4458=ORIENTED_EDGE('',*,*,#3248,.T.);
#4459=ORIENTED_EDGE('',*,*,#3249,.T.);
#4460=ORIENTED_EDGE('',*,*,#3250,.T.);
#4461=ORIENTED_EDGE('',*,*,#3251,.T.);
#4462=ORIENTED_EDGE('',*,*,#3252,.T.);
#4463=ORIENTED_EDGE('',*,*,#3245,.F.);
#4464=ORIENTED_EDGE('',*,*,#3253,.F.);
#4465=ORIENTED_EDGE('',*,*,#3252,.F.);
#4466=ORIENTED_EDGE('',*,*,#3254,.F.);
#4467=ORIENTED_EDGE('',*,*,#3255,.T.);
#4468=ORIENTED_EDGE('',*,*,#3256,.T.);
#4469=ORIENTED_EDGE('',*,*,#3257,.T.);
#4470=ORIENTED_EDGE('',*,*,#3258,.F.);
#4471=ORIENTED_EDGE('',*,*,#3259,.F.);
#4472=ORIENTED_EDGE('',*,*,#3260,.F.);
#4473=ORIENTED_EDGE('',*,*,#3257,.F.);
#4474=ORIENTED_EDGE('',*,*,#3251,.F.);
#4475=ORIENTED_EDGE('',*,*,#3261,.F.);
#4476=ORIENTED_EDGE('',*,*,#3256,.F.);
#4477=ORIENTED_EDGE('',*,*,#3262,.F.);
#4478=ORIENTED_EDGE('',*,*,#3255,.F.);
#4479=ORIENTED_EDGE('',*,*,#3263,.F.);
#4480=ORIENTED_EDGE('',*,*,#3249,.F.);
#4481=ORIENTED_EDGE('',*,*,#3264,.F.);
#4482=ORIENTED_EDGE('',*,*,#3265,.F.);
#4483=ORIENTED_EDGE('',*,*,#3266,.F.);
#4484=ORIENTED_EDGE('',*,*,#3267,.F.);
#4485=ORIENTED_EDGE('',*,*,#3250,.F.);
#4486=ORIENTED_EDGE('',*,*,#3248,.F.);
#4487=ORIENTED_EDGE('',*,*,#3268,.F.);
#4488=ORIENTED_EDGE('',*,*,#3246,.F.);
#4489=ORIENTED_EDGE('',*,*,#3269,.F.);
#4490=ORIENTED_EDGE('',*,*,#3270,.F.);
#4491=ORIENTED_EDGE('',*,*,#3271,.F.);
#4492=ORIENTED_EDGE('',*,*,#3272,.F.);
#4493=ORIENTED_EDGE('',*,*,#3247,.F.);
#4494=ORIENTED_EDGE('',*,*,#3273,.F.);
#4495=ORIENTED_EDGE('',*,*,#3242,.T.);
#4496=ORIENTED_EDGE('',*,*,#3274,.F.);
#4497=ORIENTED_EDGE('',*,*,#3259,.T.);
#4498=ORIENTED_EDGE('',*,*,#3275,.F.);
#4499=ORIENTED_EDGE('',*,*,#3276,.F.);
#4500=ORIENTED_EDGE('',*,*,#3277,.F.);
#4501=ORIENTED_EDGE('',*,*,#3244,.F.);
#4502=ORIENTED_EDGE('',*,*,#3278,.F.);
#4503=ORIENTED_EDGE('',*,*,#3239,.T.);
#4504=ORIENTED_EDGE('',*,*,#3279,.F.);
#4505=ORIENTED_EDGE('',*,*,#3266,.T.);
#4506=ORIENTED_EDGE('',*,*,#3280,.F.);
#4507=ORIENTED_EDGE('',*,*,#3236,.T.);
#4508=ORIENTED_EDGE('',*,*,#3281,.F.);
#4509=ORIENTED_EDGE('',*,*,#3271,.T.);
#4510=ORIENTED_EDGE('',*,*,#3282,.F.);
#4511=ORIENTED_EDGE('',*,*,#3226,.T.);
#4512=ORIENTED_EDGE('',*,*,#3283,.F.);
#4513=ORIENTED_EDGE('',*,*,#3276,.T.);
#4514=ORIENTED_EDGE('',*,*,#3223,.F.);
#4515=ORIENTED_EDGE('',*,*,#3284,.F.);
#4516=ORIENTED_EDGE('',*,*,#3203,.F.);
#4517=ORIENTED_EDGE('',*,*,#3285,.F.);
#4518=ORIENTED_EDGE('',*,*,#3208,.F.);
#4519=ORIENTED_EDGE('',*,*,#3286,.F.);
#4520=ORIENTED_EDGE('',*,*,#3220,.F.);
#4521=ORIENTED_EDGE('',*,*,#3287,.F.);
#4522=ORIENTED_EDGE('',*,*,#3219,.F.);
#4523=ORIENTED_EDGE('',*,*,#3288,.F.);
#4524=ORIENTED_EDGE('',*,*,#3198,.F.);
#4525=ORIENTED_EDGE('',*,*,#3289,.F.);
#4526=ORIENTED_EDGE('',*,*,#3197,.F.);
#4527=ORIENTED_EDGE('',*,*,#3290,.F.);
#4528=ORIENTED_EDGE('',*,*,#3189,.F.);
#4529=ORIENTED_EDGE('',*,*,#3291,.F.);
#4530=ORIENTED_EDGE('',*,*,#3194,.F.);
#4531=ORIENTED_EDGE('',*,*,#3115,.F.);
#4532=ORIENTED_EDGE('',*,*,#3177,.F.);
#4533=ORIENTED_EDGE('',*,*,#3292,.F.);
#4534=ORIENTED_EDGE('',*,*,#3186,.F.);
#4535=ORIENTED_EDGE('',*,*,#3116,.F.);
#4536=ORIENTED_EDGE('',*,*,#3193,.F.);
#4537=ORIENTED_EDGE('',*,*,#3293,.F.);
#4538=ORIENTED_EDGE('',*,*,#3171,.F.);
#4539=ORIENTED_EDGE('',*,*,#3117,.F.);
#4540=ORIENTED_EDGE('',*,*,#3185,.F.);
#4541=ORIENTED_EDGE('',*,*,#3294,.F.);
#4542=ORIENTED_EDGE('',*,*,#3182,.F.);
#4543=ORIENTED_EDGE('',*,*,#3129,.F.);
#4544=ORIENTED_EDGE('',*,*,#3172,.F.);
#4545=ORIENTED_EDGE('',*,*,#3295,.F.);
#4546=ORIENTED_EDGE('',*,*,#3181,.F.);
#4547=ORIENTED_EDGE('',*,*,#3296,.F.);
#4548=ORIENTED_EDGE('',*,*,#3165,.F.);
#4549=ORIENTED_EDGE('',*,*,#3130,.F.);
#4550=ORIENTED_EDGE('',*,*,#3176,.F.);
#4551=ORIENTED_EDGE('',*,*,#3297,.F.);
#4552=ORIENTED_EDGE('',*,*,#3157,.F.);
#4553=ORIENTED_EDGE('',*,*,#3298,.F.);
#4554=ORIENTED_EDGE('',*,*,#3152,.F.);
#4555=ORIENTED_EDGE('',*,*,#3299,.F.);
#4556=ORIENTED_EDGE('',*,*,#3173,.F.);
#4557=ORIENTED_EDGE('',*,*,#3132,.F.);
#4558=ORIENTED_EDGE('',*,*,#3169,.F.);
#4559=ORIENTED_EDGE('',*,*,#3300,.F.);
#4560=ORIENTED_EDGE('',*,*,#3148,.F.);
#4561=ORIENTED_EDGE('',*,*,#3301,.F.);
#4562=ORIENTED_EDGE('',*,*,#3164,.F.);
#4563=ORIENTED_EDGE('',*,*,#3302,.F.);
#4564=ORIENTED_EDGE('',*,*,#3153,.F.);
#4565=ORIENTED_EDGE('',*,*,#3131,.F.);
#4566=ORIENTED_EDGE('',*,*,#3142,.F.);
#4567=ORIENTED_EDGE('',*,*,#3303,.F.);
#4568=ORIENTED_EDGE('',*,*,#3144,.F.);
#4569=ORIENTED_EDGE('',*,*,#3304,.F.);
#4570=ORIENTED_EDGE('',*,*,#3267,.T.);
#4571=ORIENTED_EDGE('',*,*,#3305,.T.);
#4572=ORIENTED_EDGE('',*,*,#3258,.T.);
#4573=ORIENTED_EDGE('',*,*,#3261,.T.);
#4574=ORIENTED_EDGE('',*,*,#3279,.T.);
#4575=ORIENTED_EDGE('',*,*,#3306,.T.);
#4576=ORIENTED_EDGE('',*,*,#3273,.T.);
#4577=ORIENTED_EDGE('',*,*,#3305,.F.);
#4578=ORIENTED_EDGE('',*,*,#3281,.T.);
#4579=ORIENTED_EDGE('',*,*,#3307,.F.);
#4580=ORIENTED_EDGE('',*,*,#3282,.T.);
#4581=ORIENTED_EDGE('',*,*,#3308,.T.);
#4582=ORIENTED_EDGE('',*,*,#3272,.T.);
#4583=ORIENTED_EDGE('',*,*,#3308,.F.);
#4584=ORIENTED_EDGE('',*,*,#3275,.T.);
#4585=ORIENTED_EDGE('',*,*,#3268,.T.);
#4586=ORIENTED_EDGE('',*,*,#3160,.T.);
#4587=ORIENTED_EDGE('',*,*,#3162,.T.);
#4588=ORIENTED_EDGE('',*,*,#3151,.T.);
#4589=ORIENTED_EDGE('',*,*,#3304,.T.);
#4590=ORIENTED_EDGE('',*,*,#3140,.F.);
#4591=ORIENTED_EDGE('',*,*,#3135,.F.);
#4592=ORIENTED_EDGE('',*,*,#3124,.T.);
#4593=ORIENTED_EDGE('',*,*,#3120,.T.);
#4594=ORIENTED_EDGE('',*,*,#3168,.T.);
#4595=ORIENTED_EDGE('',*,*,#3303,.T.);
#4596=ORIENTED_EDGE('',*,*,#3155,.T.);
#4597=ORIENTED_EDGE('',*,*,#3302,.T.);
#4598=ORIENTED_EDGE('',*,*,#3179,.T.);
#4599=ORIENTED_EDGE('',*,*,#3301,.T.);
#4600=ORIENTED_EDGE('',*,*,#3163,.T.);
#4601=ORIENTED_EDGE('',*,*,#3297,.T.);
#4602=ORIENTED_EDGE('',*,*,#3201,.T.);
#4603=ORIENTED_EDGE('',*,*,#3295,.T.);
#4604=ORIENTED_EDGE('',*,*,#3192,.T.);
#4605=ORIENTED_EDGE('',*,*,#3290,.T.);
#4606=ORIENTED_EDGE('',*,*,#3211,.T.);
#4607=ORIENTED_EDGE('',*,*,#3287,.T.);
#4608=ORIENTED_EDGE('',*,*,#3289,.T.);
#4609=ORIENTED_EDGE('',*,*,#3291,.T.);
#4610=ORIENTED_EDGE('',*,*,#3215,.T.);
#4611=ORIENTED_EDGE('',*,*,#3217,.T.);
#4612=ORIENTED_EDGE('',*,*,#3206,.T.);
#4613=ORIENTED_EDGE('',*,*,#3293,.T.);
#4614=ORIENTED_EDGE('',*,*,#3218,.T.);
#4615=ORIENTED_EDGE('',*,*,#3232,.T.);
#4616=ORIENTED_EDGE('',*,*,#3234,.T.);
#4617=ORIENTED_EDGE('',*,*,#3285,.T.);
#4618=ORIENTED_EDGE('',*,*,#3253,.T.);
#4619=ORIENTED_EDGE('',*,*,#3277,.T.);
#4620=ORIENTED_EDGE('',*,*,#3283,.T.);
#4621=ORIENTED_EDGE('',*,*,#3225,.T.);
#4622=ORIENTED_EDGE('',*,*,#3210,.T.);
#4623=ORIENTED_EDGE('',*,*,#3191,.T.);
#4624=ORIENTED_EDGE('',*,*,#3174,.T.);
#4625=ORIENTED_EDGE('',*,*,#3299,.T.);
#4626=ORIENTED_EDGE('',*,*,#3156,.T.);
#4627=ORIENTED_EDGE('',*,*,#3150,.T.);
#4628=ORIENTED_EDGE('',*,*,#3300,.T.);
#4629=ORIENTED_EDGE('',*,*,#3294,.T.);
#4630=ORIENTED_EDGE('',*,*,#3184,.T.);
#4631=ORIENTED_EDGE('',*,*,#3205,.T.);
#4632=ORIENTED_EDGE('',*,*,#3284,.T.);
#4633=ORIENTED_EDGE('',*,*,#3240,.T.);
#4634=ORIENTED_EDGE('',*,*,#3278,.T.);
#4635=ORIENTED_EDGE('',*,*,#3265,.T.);
#4636=ORIENTED_EDGE('',*,*,#3254,.T.);
#4637=ORIENTED_EDGE('',*,*,#3262,.T.);
#4638=ORIENTED_EDGE('',*,*,#3264,.T.);
#4639=ORIENTED_EDGE('',*,*,#3269,.T.);
#4640=ORIENTED_EDGE('',*,*,#3260,.T.);
#4641=ORIENTED_EDGE('',*,*,#3274,.T.);
#4642=ORIENTED_EDGE('',*,*,#3241,.T.);
#4643=ORIENTED_EDGE('',*,*,#3231,.T.);
#4644=ORIENTED_EDGE('',*,*,#3216,.T.);
#4645=ORIENTED_EDGE('',*,*,#3195,.T.);
#4646=ORIENTED_EDGE('',*,*,#3292,.T.);
#4647=ORIENTED_EDGE('',*,*,#3298,.T.);
#4648=ORIENTED_EDGE('',*,*,#3161,.T.);
#4649=ORIENTED_EDGE('',*,*,#3167,.T.);
#4650=ORIENTED_EDGE('',*,*,#3296,.T.);
#4651=ORIENTED_EDGE('',*,*,#3180,.T.);
#4652=ORIENTED_EDGE('',*,*,#3200,.T.);
#4653=ORIENTED_EDGE('',*,*,#3288,.T.);
#4654=ORIENTED_EDGE('',*,*,#3237,.T.);
#4655=ORIENTED_EDGE('',*,*,#3280,.T.);
#4656=ORIENTED_EDGE('',*,*,#3270,.T.);
#4657=ORIENTED_EDGE('',*,*,#3263,.T.);
#4658=ORIENTED_EDGE('',*,*,#3238,.T.);
#4659=ORIENTED_EDGE('',*,*,#3233,.T.);
#4660=ORIENTED_EDGE('',*,*,#3243,.T.);
#4661=ORIENTED_EDGE('',*,*,#3306,.F.);
#4662=ORIENTED_EDGE('',*,*,#3235,.T.);
#4663=ORIENTED_EDGE('',*,*,#3286,.T.);
#4664=ORIENTED_EDGE('',*,*,#3227,.T.);
#4665=ORIENTED_EDGE('',*,*,#3307,.T.);
#4666=ORIENTED_EDGE('',*,*,#3309,.T.);
#4667=ORIENTED_EDGE('',*,*,#3310,.F.);
#4668=ORIENTED_EDGE('',*,*,#3311,.T.);
#4669=ORIENTED_EDGE('',*,*,#3309,.F.);
#4670=ORIENTED_EDGE('',*,*,#3311,.F.);
#4671=ORIENTED_EDGE('',*,*,#3310,.T.);
#4672=ORIENTED_EDGE('',*,*,#3312,.F.);
#4673=ORIENTED_EDGE('',*,*,#3313,.T.);
#4674=ORIENTED_EDGE('',*,*,#3314,.F.);
#4675=ORIENTED_EDGE('',*,*,#3315,.F.);
#4676=ORIENTED_EDGE('',*,*,#3313,.F.);
#4677=ORIENTED_EDGE('',*,*,#3316,.T.);
#4678=ORIENTED_EDGE('',*,*,#3312,.T.);
#4679=ORIENTED_EDGE('',*,*,#3314,.T.);
#4680=ORIENTED_EDGE('',*,*,#3315,.T.);
#4681=ORIENTED_EDGE('',*,*,#3317,.T.);
#4682=ORIENTED_EDGE('',*,*,#3318,.T.);
#4683=ORIENTED_EDGE('',*,*,#3319,.T.);
#4684=ORIENTED_EDGE('',*,*,#3317,.F.);
#4685=ORIENTED_EDGE('',*,*,#3316,.F.);
#4686=ORIENTED_EDGE('',*,*,#3320,.T.);
#4687=ORIENTED_EDGE('',*,*,#3321,.F.);
#4688=ORIENTED_EDGE('',*,*,#3322,.F.);
#4689=ORIENTED_EDGE('',*,*,#3320,.F.);
#4690=ORIENTED_EDGE('',*,*,#3321,.T.);
#4691=ORIENTED_EDGE('',*,*,#3322,.T.);
#4692=ORIENTED_EDGE('',*,*,#3323,.T.);
#4693=ORIENTED_EDGE('',*,*,#3324,.T.);
#4694=ORIENTED_EDGE('',*,*,#3325,.T.);
#4695=ORIENTED_EDGE('',*,*,#3323,.F.);
#4696=ORIENTED_EDGE('',*,*,#3326,.F.);
#4697=ORIENTED_EDGE('',*,*,#3327,.T.);
#4698=ORIENTED_EDGE('',*,*,#3318,.F.);
#4699=ORIENTED_EDGE('',*,*,#3319,.F.);
#4700=ORIENTED_EDGE('',*,*,#3327,.F.);
#4701=ORIENTED_EDGE('',*,*,#3328,.T.);
#4702=ORIENTED_EDGE('',*,*,#3326,.T.);
#4703=ORIENTED_EDGE('',*,*,#3328,.F.);
#4704=ORIENTED_EDGE('',*,*,#3329,.T.);
#4705=ORIENTED_EDGE('',*,*,#3324,.F.);
#4706=ORIENTED_EDGE('',*,*,#3325,.F.);
#4707=ORIENTED_EDGE('',*,*,#3329,.F.);
#4708=ORIENTED_EDGE('',*,*,#3330,.F.);
#4709=ORIENTED_EDGE('',*,*,#3331,.T.);
#4710=ORIENTED_EDGE('',*,*,#3332,.T.);
#4711=ORIENTED_EDGE('',*,*,#3330,.T.);
#4712=ORIENTED_EDGE('',*,*,#3332,.F.);
#4713=ORIENTED_EDGE('',*,*,#3331,.F.);
#4714=ORIENTED_EDGE('',*,*,#3333,.T.);
#4715=ORIENTED_EDGE('',*,*,#3334,.F.);
#4716=ORIENTED_EDGE('',*,*,#3335,.T.);
#4717=ORIENTED_EDGE('',*,*,#3333,.F.);
#4718=ORIENTED_EDGE('',*,*,#3335,.F.);
#4719=ORIENTED_EDGE('',*,*,#3334,.T.);
#4720=ORIENTED_EDGE('',*,*,#3336,.T.);
#4721=ORIENTED_EDGE('',*,*,#3337,.T.);
#4722=ORIENTED_EDGE('',*,*,#3338,.T.);
#4723=ORIENTED_EDGE('',*,*,#3339,.T.);
#4724=ORIENTED_EDGE('',*,*,#3337,.F.);
#4725=ORIENTED_EDGE('',*,*,#3340,.F.);
#4726=ORIENTED_EDGE('',*,*,#3336,.F.);
#4727=ORIENTED_EDGE('',*,*,#3339,.F.);
#4728=ORIENTED_EDGE('',*,*,#3341,.T.);
#4729=ORIENTED_EDGE('',*,*,#3342,.F.);
#4730=ORIENTED_EDGE('',*,*,#3343,.F.);
#4731=ORIENTED_EDGE('',*,*,#3341,.F.);
#4732=ORIENTED_EDGE('',*,*,#3338,.F.);
#4733=ORIENTED_EDGE('',*,*,#3340,.T.);
#4734=ORIENTED_EDGE('',*,*,#3344,.T.);
#4735=ORIENTED_EDGE('',*,*,#3345,.T.);
#4736=ORIENTED_EDGE('',*,*,#3346,.T.);
#4737=ORIENTED_EDGE('',*,*,#3344,.F.);
#4738=ORIENTED_EDGE('',*,*,#3346,.F.);
#4739=ORIENTED_EDGE('',*,*,#3347,.T.);
#4740=ORIENTED_EDGE('',*,*,#3348,.F.);
#4741=ORIENTED_EDGE('',*,*,#3349,.F.);
#4742=ORIENTED_EDGE('',*,*,#3347,.F.);
#4743=ORIENTED_EDGE('',*,*,#3345,.F.);
#4744=ORIENTED_EDGE('',*,*,#3350,.T.);
#4745=ORIENTED_EDGE('',*,*,#3351,.T.);
#4746=ORIENTED_EDGE('',*,*,#3342,.T.);
#4747=ORIENTED_EDGE('',*,*,#3343,.T.);
#4748=ORIENTED_EDGE('',*,*,#3351,.F.);
#4749=ORIENTED_EDGE('',*,*,#3352,.F.);
#4750=ORIENTED_EDGE('',*,*,#3350,.F.);
#4751=ORIENTED_EDGE('',*,*,#3352,.T.);
#4752=ORIENTED_EDGE('',*,*,#3353,.T.);
#4753=ORIENTED_EDGE('',*,*,#3348,.T.);
#4754=ORIENTED_EDGE('',*,*,#3349,.T.);
#4755=ORIENTED_EDGE('',*,*,#3353,.F.);
#4756=ORIENTED_EDGE('',*,*,#3354,.T.);
#4757=ORIENTED_EDGE('',*,*,#3355,.T.);
#4758=ORIENTED_EDGE('',*,*,#3356,.T.);
#4759=ORIENTED_EDGE('',*,*,#3355,.F.);
#4760=ORIENTED_EDGE('',*,*,#3357,.F.);
#4761=ORIENTED_EDGE('',*,*,#3358,.F.);
#4762=ORIENTED_EDGE('',*,*,#3359,.F.);
#4763=ORIENTED_EDGE('',*,*,#3360,.F.);
#4764=ORIENTED_EDGE('',*,*,#3361,.F.);
#4765=ORIENTED_EDGE('',*,*,#3356,.F.);
#4766=ORIENTED_EDGE('',*,*,#3354,.F.);
#4767=ORIENTED_EDGE('',*,*,#3362,.T.);
#4768=ORIENTED_EDGE('',*,*,#3363,.T.);
#4769=ORIENTED_EDGE('',*,*,#3362,.F.);
#4770=ORIENTED_EDGE('',*,*,#3364,.T.);
#4771=ORIENTED_EDGE('',*,*,#3365,.T.);
#4772=ORIENTED_EDGE('',*,*,#3361,.T.);
#4773=ORIENTED_EDGE('',*,*,#3365,.F.);
#4774=ORIENTED_EDGE('',*,*,#3364,.F.);
#4775=ORIENTED_EDGE('',*,*,#3366,.T.);
#4776=ORIENTED_EDGE('',*,*,#3367,.T.);
#4777=ORIENTED_EDGE('',*,*,#3366,.F.);
#4778=ORIENTED_EDGE('',*,*,#3368,.T.);
#4779=ORIENTED_EDGE('',*,*,#3369,.T.);
#4780=ORIENTED_EDGE('',*,*,#3370,.T.);
#4781=ORIENTED_EDGE('',*,*,#3371,.T.);
#4782=ORIENTED_EDGE('',*,*,#3369,.F.);
#4783=ORIENTED_EDGE('',*,*,#3372,.F.);
#4784=ORIENTED_EDGE('',*,*,#3373,.F.);
#4785=ORIENTED_EDGE('',*,*,#3374,.F.);
#4786=ORIENTED_EDGE('',*,*,#3375,.F.);
#4787=ORIENTED_EDGE('',*,*,#3376,.F.);
#4788=ORIENTED_EDGE('',*,*,#3368,.F.);
#4789=ORIENTED_EDGE('',*,*,#3371,.F.);
#4790=ORIENTED_EDGE('',*,*,#3377,.T.);
#4791=ORIENTED_EDGE('',*,*,#3378,.F.);
#4792=ORIENTED_EDGE('',*,*,#3377,.F.);
#4793=ORIENTED_EDGE('',*,*,#3370,.F.);
#4794=ORIENTED_EDGE('',*,*,#3376,.T.);
#4795=ORIENTED_EDGE('',*,*,#3379,.T.);
#4796=ORIENTED_EDGE('',*,*,#3380,.T.);
#4797=ORIENTED_EDGE('',*,*,#3381,.T.);
#4798=ORIENTED_EDGE('',*,*,#3379,.F.);
#4799=ORIENTED_EDGE('',*,*,#3381,.F.);
#4800=ORIENTED_EDGE('',*,*,#3382,.T.);
#4801=ORIENTED_EDGE('',*,*,#3383,.F.);
#4802=ORIENTED_EDGE('',*,*,#3382,.F.);
#4803=ORIENTED_EDGE('',*,*,#3380,.F.);
#4804=ORIENTED_EDGE('',*,*,#3384,.F.);
#4805=ORIENTED_EDGE('',*,*,#3385,.F.);
#4806=ORIENTED_EDGE('',*,*,#3386,.F.);
#4807=ORIENTED_EDGE('',*,*,#3387,.F.);
#4808=ORIENTED_EDGE('',*,*,#3388,.F.);
#4809=ORIENTED_EDGE('',*,*,#3389,.F.);
#4810=ORIENTED_EDGE('',*,*,#3390,.F.);
#4811=ORIENTED_EDGE('',*,*,#3391,.F.);
#4812=ORIENTED_EDGE('',*,*,#3392,.F.);
#4813=ORIENTED_EDGE('',*,*,#3391,.T.);
#4814=ORIENTED_EDGE('',*,*,#3393,.T.);
#4815=ORIENTED_EDGE('',*,*,#3385,.T.);
#4816=ORIENTED_EDGE('',*,*,#3394,.T.);
#4817=ORIENTED_EDGE('',*,*,#3395,.F.);
#4818=ORIENTED_EDGE('',*,*,#3396,.F.);
#4819=ORIENTED_EDGE('',*,*,#3397,.F.);
#4820=ORIENTED_EDGE('',*,*,#3396,.T.);
#4821=ORIENTED_EDGE('',*,*,#3398,.T.);
#4822=ORIENTED_EDGE('',*,*,#3384,.T.);
#4823=ORIENTED_EDGE('',*,*,#3399,.T.);
#4824=ORIENTED_EDGE('',*,*,#3400,.F.);
#4825=ORIENTED_EDGE('',*,*,#3401,.F.);
#4826=ORIENTED_EDGE('',*,*,#3402,.F.);
#4827=ORIENTED_EDGE('',*,*,#3401,.T.);
#4828=ORIENTED_EDGE('',*,*,#3403,.T.);
#4829=ORIENTED_EDGE('',*,*,#3388,.T.);
#4830=ORIENTED_EDGE('',*,*,#3404,.T.);
#4831=ORIENTED_EDGE('',*,*,#3390,.T.);
#4832=ORIENTED_EDGE('',*,*,#3405,.T.);
#4833=ORIENTED_EDGE('',*,*,#3402,.T.);
#4834=ORIENTED_EDGE('',*,*,#3406,.T.);
#4835=ORIENTED_EDGE('',*,*,#3407,.F.);
#4836=ORIENTED_EDGE('',*,*,#3408,.F.);
#4837=ORIENTED_EDGE('',*,*,#3409,.F.);
#4838=ORIENTED_EDGE('',*,*,#3408,.T.);
#4839=ORIENTED_EDGE('',*,*,#3410,.T.);
#4840=ORIENTED_EDGE('',*,*,#3389,.T.);
#4841=ORIENTED_EDGE('',*,*,#3411,.T.);
#4842=ORIENTED_EDGE('',*,*,#3412,.F.);
#4843=ORIENTED_EDGE('',*,*,#3413,.F.);
#4844=ORIENTED_EDGE('',*,*,#3414,.F.);
#4845=ORIENTED_EDGE('',*,*,#3415,.F.);
#4846=ORIENTED_EDGE('',*,*,#3416,.F.);
#4847=ORIENTED_EDGE('',*,*,#3417,.T.);
#4848=ORIENTED_EDGE('',*,*,#3418,.F.);
#4849=ORIENTED_EDGE('',*,*,#3419,.F.);
#4850=ORIENTED_EDGE('',*,*,#3420,.F.);
#4851=ORIENTED_EDGE('',*,*,#3421,.F.);
#4852=ORIENTED_EDGE('',*,*,#3420,.T.);
#4853=ORIENTED_EDGE('',*,*,#3422,.T.);
#4854=ORIENTED_EDGE('',*,*,#3414,.T.);
#4855=ORIENTED_EDGE('',*,*,#3357,.T.);
#4856=ORIENTED_EDGE('',*,*,#3423,.T.);
#4857=ORIENTED_EDGE('',*,*,#3424,.F.);
#4858=ORIENTED_EDGE('',*,*,#3425,.F.);
#4859=ORIENTED_EDGE('',*,*,#3426,.F.);
#4860=ORIENTED_EDGE('',*,*,#3427,.T.);
#4861=ORIENTED_EDGE('',*,*,#3428,.F.);
#4862=ORIENTED_EDGE('',*,*,#3429,.F.);
#4863=ORIENTED_EDGE('',*,*,#3430,.F.);
#4864=ORIENTED_EDGE('',*,*,#3431,.F.);
#4865=ORIENTED_EDGE('',*,*,#3432,.F.);
#4866=ORIENTED_EDGE('',*,*,#3433,.F.);
#4867=ORIENTED_EDGE('',*,*,#3416,.T.);
#4868=ORIENTED_EDGE('',*,*,#3434,.T.);
#4869=ORIENTED_EDGE('',*,*,#3432,.T.);
#4870=ORIENTED_EDGE('',*,*,#3435,.T.);
#4871=ORIENTED_EDGE('',*,*,#3436,.F.);
#4872=ORIENTED_EDGE('',*,*,#3437,.F.);
#4873=ORIENTED_EDGE('',*,*,#3438,.T.);
#4874=ORIENTED_EDGE('',*,*,#3439,.F.);
#4875=ORIENTED_EDGE('',*,*,#3440,.F.);
#4876=ORIENTED_EDGE('',*,*,#3441,.F.);
#4877=ORIENTED_EDGE('',*,*,#3442,.F.);
#4878=ORIENTED_EDGE('',*,*,#3441,.T.);
#4879=ORIENTED_EDGE('',*,*,#3443,.T.);
#4880=ORIENTED_EDGE('',*,*,#3424,.T.);
#4881=ORIENTED_EDGE('',*,*,#3444,.T.);
#4882=ORIENTED_EDGE('',*,*,#3445,.F.);
#4883=ORIENTED_EDGE('',*,*,#3446,.F.);
#4884=ORIENTED_EDGE('',*,*,#3447,.F.);
#4885=ORIENTED_EDGE('',*,*,#3446,.T.);
#4886=ORIENTED_EDGE('',*,*,#3448,.T.);
#4887=ORIENTED_EDGE('',*,*,#3428,.T.);
#4888=ORIENTED_EDGE('',*,*,#3449,.T.);
#4889=ORIENTED_EDGE('',*,*,#3450,.F.);
#4890=ORIENTED_EDGE('',*,*,#3451,.F.);
#4891=ORIENTED_EDGE('',*,*,#3452,.F.);
#4892=ORIENTED_EDGE('',*,*,#3431,.T.);
#4893=ORIENTED_EDGE('',*,*,#3453,.T.);
#4894=ORIENTED_EDGE('',*,*,#3451,.T.);
#4895=ORIENTED_EDGE('',*,*,#3454,.T.);
#4896=ORIENTED_EDGE('',*,*,#3455,.F.);
#4897=ORIENTED_EDGE('',*,*,#3456,.F.);
#4898=ORIENTED_EDGE('',*,*,#3457,.F.);
#4899=ORIENTED_EDGE('',*,*,#3456,.T.);
#4900=ORIENTED_EDGE('',*,*,#3458,.T.);
#4901=ORIENTED_EDGE('',*,*,#3437,.T.);
#4902=ORIENTED_EDGE('',*,*,#3459,.T.);
#4903=ORIENTED_EDGE('',*,*,#3445,.T.);
#4904=ORIENTED_EDGE('',*,*,#3460,.T.);
#4905=ORIENTED_EDGE('',*,*,#3457,.T.);
#4906=ORIENTED_EDGE('',*,*,#3461,.T.);
#4907=ORIENTED_EDGE('',*,*,#3462,.F.);
#4908=ORIENTED_EDGE('',*,*,#3463,.F.);
#4909=ORIENTED_EDGE('',*,*,#3464,.F.);
#4910=ORIENTED_EDGE('',*,*,#3465,.F.);
#4911=ORIENTED_EDGE('',*,*,#3466,.F.);
#4912=ORIENTED_EDGE('',*,*,#3467,.F.);
#4913=ORIENTED_EDGE('',*,*,#3468,.T.);
#4914=ORIENTED_EDGE('',*,*,#3450,.T.);
#4915=ORIENTED_EDGE('',*,*,#3469,.T.);
#4916=ORIENTED_EDGE('',*,*,#3470,.T.);
#4917=ORIENTED_EDGE('',*,*,#3471,.F.);
#4918=ORIENTED_EDGE('',*,*,#3472,.F.);
#4919=ORIENTED_EDGE('',*,*,#3473,.F.);
#4920=ORIENTED_EDGE('',*,*,#3455,.T.);
#4921=ORIENTED_EDGE('',*,*,#3474,.T.);
#4922=ORIENTED_EDGE('',*,*,#3472,.T.);
#4923=ORIENTED_EDGE('',*,*,#3475,.T.);
#4924=ORIENTED_EDGE('',*,*,#3473,.T.);
#4925=ORIENTED_EDGE('',*,*,#3476,.T.);
#4926=ORIENTED_EDGE('',*,*,#3466,.T.);
#4927=ORIENTED_EDGE('',*,*,#3477,.T.);
#4928=ORIENTED_EDGE('',*,*,#3478,.T.);
#4929=ORIENTED_EDGE('',*,*,#3463,.T.);
#4930=ORIENTED_EDGE('',*,*,#3479,.T.);
#4931=ORIENTED_EDGE('',*,*,#3480,.T.);
#4932=ORIENTED_EDGE('',*,*,#3481,.T.);
#4933=ORIENTED_EDGE('',*,*,#3465,.T.);
#4934=ORIENTED_EDGE('',*,*,#3482,.T.);
#4935=ORIENTED_EDGE('',*,*,#3483,.T.);
#4936=ORIENTED_EDGE('',*,*,#3484,.T.);
#4937=ORIENTED_EDGE('',*,*,#3471,.T.);
#4938=ORIENTED_EDGE('',*,*,#3485,.T.);
#4939=ORIENTED_EDGE('',*,*,#3486,.T.);
#4940=ORIENTED_EDGE('',*,*,#3487,.F.);
#4941=ORIENTED_EDGE('',*,*,#3488,.F.);
#4942=ORIENTED_EDGE('',*,*,#3489,.F.);
#4943=ORIENTED_EDGE('',*,*,#3490,.F.);
#4944=ORIENTED_EDGE('',*,*,#3491,.F.);
#4945=ORIENTED_EDGE('',*,*,#3492,.F.);
#4946=ORIENTED_EDGE('',*,*,#3493,.F.);
#4947=ORIENTED_EDGE('',*,*,#3494,.F.);
#4948=ORIENTED_EDGE('',*,*,#3495,.F.);
#4949=ORIENTED_EDGE('',*,*,#3489,.T.);
#4950=ORIENTED_EDGE('',*,*,#3496,.T.);
#4951=ORIENTED_EDGE('',*,*,#3494,.T.);
#4952=ORIENTED_EDGE('',*,*,#3497,.T.);
#4953=ORIENTED_EDGE('',*,*,#3498,.F.);
#4954=ORIENTED_EDGE('',*,*,#3499,.F.);
#4955=ORIENTED_EDGE('',*,*,#3500,.F.);
#4956=ORIENTED_EDGE('',*,*,#3501,.T.);
#4957=ORIENTED_EDGE('',*,*,#3499,.T.);
#4958=ORIENTED_EDGE('',*,*,#3502,.T.);
#4959=ORIENTED_EDGE('',*,*,#3503,.T.);
#4960=ORIENTED_EDGE('',*,*,#3495,.T.);
#4961=ORIENTED_EDGE('',*,*,#3504,.T.);
#4962=ORIENTED_EDGE('',*,*,#3500,.T.);
#4963=ORIENTED_EDGE('',*,*,#3505,.T.);
#4964=ORIENTED_EDGE('',*,*,#3498,.T.);
#4965=ORIENTED_EDGE('',*,*,#3506,.T.);
#4966=ORIENTED_EDGE('',*,*,#3491,.T.);
#4967=ORIENTED_EDGE('',*,*,#3507,.T.);
#4968=ORIENTED_EDGE('',*,*,#3508,.T.);
#4969=ORIENTED_EDGE('',*,*,#3493,.T.);
#4970=ORIENTED_EDGE('',*,*,#3509,.T.);
#4971=ORIENTED_EDGE('',*,*,#3510,.T.);
#4972=ORIENTED_EDGE('',*,*,#3492,.T.);
#4973=ORIENTED_EDGE('',*,*,#3511,.T.);
#4974=ORIENTED_EDGE('',*,*,#3488,.T.);
#4975=ORIENTED_EDGE('',*,*,#3512,.T.);
#4976=ORIENTED_EDGE('',*,*,#3513,.T.);
#4977=ORIENTED_EDGE('',*,*,#3490,.T.);
#4978=ORIENTED_EDGE('',*,*,#3514,.T.);
#4979=ORIENTED_EDGE('',*,*,#3515,.T.);
#4980=ORIENTED_EDGE('',*,*,#3516,.T.);
#4981=ORIENTED_EDGE('',*,*,#3503,.F.);
#4982=ORIENTED_EDGE('',*,*,#3517,.T.);
#4983=ORIENTED_EDGE('',*,*,#3486,.F.);
#4984=ORIENTED_EDGE('',*,*,#3518,.T.);
#4985=ORIENTED_EDGE('',*,*,#3487,.T.);
#4986=ORIENTED_EDGE('',*,*,#3519,.T.);
#4987=ORIENTED_EDGE('',*,*,#3520,.T.);
#4988=ORIENTED_EDGE('',*,*,#3521,.T.);
#4989=ORIENTED_EDGE('',*,*,#3510,.F.);
#4990=ORIENTED_EDGE('',*,*,#3522,.T.);
#4991=ORIENTED_EDGE('',*,*,#3483,.F.);
#4992=ORIENTED_EDGE('',*,*,#3523,.T.);
#4993=ORIENTED_EDGE('',*,*,#3515,.F.);
#4994=ORIENTED_EDGE('',*,*,#3524,.T.);
#4995=ORIENTED_EDGE('',*,*,#3480,.F.);
#4996=ORIENTED_EDGE('',*,*,#3525,.T.);
#4997=ORIENTED_EDGE('',*,*,#3520,.F.);
#4998=ORIENTED_EDGE('',*,*,#3526,.T.);
#4999=ORIENTED_EDGE('',*,*,#3470,.F.);
#5000=ORIENTED_EDGE('',*,*,#3467,.T.);
#5001=ORIENTED_EDGE('',*,*,#3527,.T.);
#5002=ORIENTED_EDGE('',*,*,#3447,.T.);
#5003=ORIENTED_EDGE('',*,*,#3528,.T.);
#5004=ORIENTED_EDGE('',*,*,#3452,.T.);
#5005=ORIENTED_EDGE('',*,*,#3529,.T.);
#5006=ORIENTED_EDGE('',*,*,#3464,.T.);
#5007=ORIENTED_EDGE('',*,*,#3530,.T.);
#5008=ORIENTED_EDGE('',*,*,#3462,.T.);
#5009=ORIENTED_EDGE('',*,*,#3531,.T.);
#5010=ORIENTED_EDGE('',*,*,#3442,.T.);
#5011=ORIENTED_EDGE('',*,*,#3532,.T.);
#5012=ORIENTED_EDGE('',*,*,#3440,.T.);
#5013=ORIENTED_EDGE('',*,*,#3533,.T.);
#5014=ORIENTED_EDGE('',*,*,#3433,.T.);
#5015=ORIENTED_EDGE('',*,*,#3534,.T.);
#5016=ORIENTED_EDGE('',*,*,#3439,.T.);
#5017=ORIENTED_EDGE('',*,*,#3535,.T.);
#5018=ORIENTED_EDGE('',*,*,#3421,.T.);
#5019=ORIENTED_EDGE('',*,*,#3360,.T.);
#5020=ORIENTED_EDGE('',*,*,#3429,.T.);
#5021=ORIENTED_EDGE('',*,*,#3536,.T.);
#5022=ORIENTED_EDGE('',*,*,#3436,.T.);
#5023=ORIENTED_EDGE('',*,*,#3359,.T.);
#5024=ORIENTED_EDGE('',*,*,#3413,.T.);
#5025=ORIENTED_EDGE('',*,*,#3537,.T.);
#5026=ORIENTED_EDGE('',*,*,#3430,.T.);
#5027=ORIENTED_EDGE('',*,*,#3358,.T.);
#5028=ORIENTED_EDGE('',*,*,#3425,.T.);
#5029=ORIENTED_EDGE('',*,*,#3538,.T.);
#5030=ORIENTED_EDGE('',*,*,#3415,.T.);
#5031=ORIENTED_EDGE('',*,*,#3372,.T.);
#5032=ORIENTED_EDGE('',*,*,#3426,.T.);
#5033=ORIENTED_EDGE('',*,*,#3375,.T.);
#5034=ORIENTED_EDGE('',*,*,#3409,.T.);
#5035=ORIENTED_EDGE('',*,*,#3539,.T.);
#5036=ORIENTED_EDGE('',*,*,#3419,.T.);
#5037=ORIENTED_EDGE('',*,*,#3540,.T.);
#5038=ORIENTED_EDGE('',*,*,#3400,.T.);
#5039=ORIENTED_EDGE('',*,*,#3541,.T.);
#5040=ORIENTED_EDGE('',*,*,#3395,.T.);
#5041=ORIENTED_EDGE('',*,*,#3373,.T.);
#5042=ORIENTED_EDGE('',*,*,#3418,.T.);
#5043=ORIENTED_EDGE('',*,*,#3542,.T.);
#5044=ORIENTED_EDGE('',*,*,#3412,.T.);
#5045=ORIENTED_EDGE('',*,*,#3543,.T.);
#5046=ORIENTED_EDGE('',*,*,#3392,.T.);
#5047=ORIENTED_EDGE('',*,*,#3544,.T.);
#5048=ORIENTED_EDGE('',*,*,#3407,.T.);
#5049=ORIENTED_EDGE('',*,*,#3374,.T.);
#5050=ORIENTED_EDGE('',*,*,#3397,.T.);
#5051=ORIENTED_EDGE('',*,*,#3545,.T.);
#5052=ORIENTED_EDGE('',*,*,#3386,.T.);
#5053=ORIENTED_EDGE('',*,*,#3546,.T.);
#5054=ORIENTED_EDGE('',*,*,#3387,.T.);
#5055=ORIENTED_EDGE('',*,*,#3547,.T.);
#5056=ORIENTED_EDGE('',*,*,#3509,.F.);
#5057=ORIENTED_EDGE('',*,*,#3505,.F.);
#5058=ORIENTED_EDGE('',*,*,#3501,.F.);
#5059=ORIENTED_EDGE('',*,*,#3548,.F.);
#5060=ORIENTED_EDGE('',*,*,#3522,.F.);
#5061=ORIENTED_EDGE('',*,*,#3548,.T.);
#5062=ORIENTED_EDGE('',*,*,#3516,.F.);
#5063=ORIENTED_EDGE('',*,*,#3549,.F.);
#5064=ORIENTED_EDGE('',*,*,#3524,.F.);
#5065=ORIENTED_EDGE('',*,*,#3550,.F.);
#5066=ORIENTED_EDGE('',*,*,#3525,.F.);
#5067=ORIENTED_EDGE('',*,*,#3551,.T.);
#5068=ORIENTED_EDGE('',*,*,#3514,.F.);
#5069=ORIENTED_EDGE('',*,*,#3512,.F.);
#5070=ORIENTED_EDGE('',*,*,#3518,.F.);
#5071=ORIENTED_EDGE('',*,*,#3550,.T.);
#5072=ORIENTED_EDGE('',*,*,#3404,.F.);
#5073=ORIENTED_EDGE('',*,*,#3546,.F.);
#5074=ORIENTED_EDGE('',*,*,#3393,.F.);
#5075=ORIENTED_EDGE('',*,*,#3406,.F.);
#5076=ORIENTED_EDGE('',*,*,#3383,.T.);
#5077=ORIENTED_EDGE('',*,*,#3378,.T.);
#5078=ORIENTED_EDGE('',*,*,#3367,.F.);
#5079=ORIENTED_EDGE('',*,*,#3363,.F.);
#5080=ORIENTED_EDGE('',*,*,#3410,.F.);
#5081=ORIENTED_EDGE('',*,*,#3545,.F.);
#5082=ORIENTED_EDGE('',*,*,#3399,.F.);
#5083=ORIENTED_EDGE('',*,*,#3547,.F.);
#5084=ORIENTED_EDGE('',*,*,#3422,.F.);
#5085=ORIENTED_EDGE('',*,*,#3541,.F.);
#5086=ORIENTED_EDGE('',*,*,#3405,.F.);
#5087=ORIENTED_EDGE('',*,*,#3543,.F.);
#5088=ORIENTED_EDGE('',*,*,#3443,.F.);
#5089=ORIENTED_EDGE('',*,*,#3534,.F.);
#5090=ORIENTED_EDGE('',*,*,#3434,.F.);
#5091=ORIENTED_EDGE('',*,*,#3538,.F.);
#5092=ORIENTED_EDGE('',*,*,#3453,.F.);
#5093=ORIENTED_EDGE('',*,*,#3533,.F.);
#5094=ORIENTED_EDGE('',*,*,#3531,.F.);
#5095=ORIENTED_EDGE('',*,*,#3529,.F.);
#5096=ORIENTED_EDGE('',*,*,#3459,.F.);
#5097=ORIENTED_EDGE('',*,*,#3536,.F.);
#5098=ORIENTED_EDGE('',*,*,#3448,.F.);
#5099=ORIENTED_EDGE('',*,*,#3461,.F.);
#5100=ORIENTED_EDGE('',*,*,#3460,.F.);
#5101=ORIENTED_EDGE('',*,*,#3527,.F.);
#5102=ORIENTED_EDGE('',*,*,#3476,.F.);
#5103=ORIENTED_EDGE('',*,*,#3474,.F.);
#5104=ORIENTED_EDGE('',*,*,#3497,.F.);
#5105=ORIENTED_EDGE('',*,*,#3508,.F.);
#5106=ORIENTED_EDGE('',*,*,#3521,.F.);
#5107=ORIENTED_EDGE('',*,*,#3482,.F.);
#5108=ORIENTED_EDGE('',*,*,#3528,.F.);
#5109=ORIENTED_EDGE('',*,*,#3449,.F.);
#5110=ORIENTED_EDGE('',*,*,#3427,.F.);
#5111=ORIENTED_EDGE('',*,*,#3537,.F.);
#5112=ORIENTED_EDGE('',*,*,#3544,.F.);
#5113=ORIENTED_EDGE('',*,*,#3394,.F.);
#5114=ORIENTED_EDGE('',*,*,#3398,.F.);
#5115=ORIENTED_EDGE('',*,*,#3542,.F.);
#5116=ORIENTED_EDGE('',*,*,#3417,.F.);
#5117=ORIENTED_EDGE('',*,*,#3435,.F.);
#5118=ORIENTED_EDGE('',*,*,#3454,.F.);
#5119=ORIENTED_EDGE('',*,*,#3468,.F.);
#5120=ORIENTED_EDGE('',*,*,#3526,.F.);
#5121=ORIENTED_EDGE('',*,*,#3519,.F.);
#5122=ORIENTED_EDGE('',*,*,#3496,.F.);
#5123=ORIENTED_EDGE('',*,*,#3511,.F.);
#5124=ORIENTED_EDGE('',*,*,#3506,.F.);
#5125=ORIENTED_EDGE('',*,*,#3504,.F.);
#5126=ORIENTED_EDGE('',*,*,#3502,.F.);
#5127=ORIENTED_EDGE('',*,*,#3507,.F.);
#5128=ORIENTED_EDGE('',*,*,#3513,.F.);
#5129=ORIENTED_EDGE('',*,*,#3523,.F.);
#5130=ORIENTED_EDGE('',*,*,#3479,.F.);
#5131=ORIENTED_EDGE('',*,*,#3532,.F.);
#5132=ORIENTED_EDGE('',*,*,#3444,.F.);
#5133=ORIENTED_EDGE('',*,*,#3423,.F.);
#5134=ORIENTED_EDGE('',*,*,#3539,.F.);
#5135=ORIENTED_EDGE('',*,*,#3411,.F.);
#5136=ORIENTED_EDGE('',*,*,#3403,.F.);
#5137=ORIENTED_EDGE('',*,*,#3540,.F.);
#5138=ORIENTED_EDGE('',*,*,#3535,.F.);
#5139=ORIENTED_EDGE('',*,*,#3438,.F.);
#5140=ORIENTED_EDGE('',*,*,#3458,.F.);
#5141=ORIENTED_EDGE('',*,*,#3475,.F.);
#5142=ORIENTED_EDGE('',*,*,#3484,.F.);
#5143=ORIENTED_EDGE('',*,*,#3517,.F.);
#5144=ORIENTED_EDGE('',*,*,#3481,.F.);
#5145=ORIENTED_EDGE('',*,*,#3549,.T.);
#5146=ORIENTED_EDGE('',*,*,#3485,.F.);
#5147=ORIENTED_EDGE('',*,*,#3477,.F.);
#5148=ORIENTED_EDGE('',*,*,#3478,.F.);
#5149=ORIENTED_EDGE('',*,*,#3551,.F.);
#5150=ORIENTED_EDGE('',*,*,#3469,.F.);
#5151=ORIENTED_EDGE('',*,*,#3530,.F.);
#5152=CYLINDRICAL_SURFACE('',#5836,5.13675);
#5153=CYLINDRICAL_SURFACE('',#5855,5.);
#5154=CYLINDRICAL_SURFACE('',#5862,5.);
#5155=CYLINDRICAL_SURFACE('',#5896,1.5);
#5156=CYLINDRICAL_SURFACE('',#5901,1.5);
#5157=CYLINDRICAL_SURFACE('',#5906,1.5);
#5158=CYLINDRICAL_SURFACE('',#5911,1.5);
#5159=CYLINDRICAL_SURFACE('',#5916,1.5);
#5160=CYLINDRICAL_SURFACE('',#5921,1.5);
#5161=CYLINDRICAL_SURFACE('',#5926,1.5);
#5162=CYLINDRICAL_SURFACE('',#5932,1.5);
#5163=CYLINDRICAL_SURFACE('',#5937,1.5);
#5164=CYLINDRICAL_SURFACE('',#5943,1.5);
#5165=CYLINDRICAL_SURFACE('',#5948,1.5);
#5166=CYLINDRICAL_SURFACE('',#5953,1.5);
#5167=CYLINDRICAL_SURFACE('',#5958,1.5);
#5168=CYLINDRICAL_SURFACE('',#5963,1.5);
#5169=CYLINDRICAL_SURFACE('',#5968,1.5);
#5170=CYLINDRICAL_SURFACE('',#5973,1.5);
#5171=CYLINDRICAL_SURFACE('',#5975,0.3);
#5172=CYLINDRICAL_SURFACE('',#5978,0.3);
#5173=CYLINDRICAL_SURFACE('',#5981,0.3);
#5174=CYLINDRICAL_SURFACE('',#5983,0.3);
#5175=CYLINDRICAL_SURFACE('',#5985,0.3);
#5176=CYLINDRICAL_SURFACE('',#5987,0.3);
#5177=CYLINDRICAL_SURFACE('',#5989,0.3);
#5178=CYLINDRICAL_SURFACE('',#5992,0.3);
#5179=CYLINDRICAL_SURFACE('',#6002,0.3);
#5180=CYLINDRICAL_SURFACE('',#6003,0.3);
#5181=CYLINDRICAL_SURFACE('',#6008,0.3);
#5182=CYLINDRICAL_SURFACE('',#6018,0.3);
#5183=CYLINDRICAL_SURFACE('',#6020,0.3);
#5184=CYLINDRICAL_SURFACE('',#6025,0.3);
#5185=CYLINDRICAL_SURFACE('',#6042,0.3);
#5186=CYLINDRICAL_SURFACE('',#6043,0.3);
#5187=CYLINDRICAL_SURFACE('',#6056,0.3);
#5188=CYLINDRICAL_SURFACE('',#6061,0.3);
#5189=CYLINDRICAL_SURFACE('',#6066,0.3);
#5190=CYLINDRICAL_SURFACE('',#6079,0.3);
#5191=CYLINDRICAL_SURFACE('',#6080,0.3);
#5192=CYLINDRICAL_SURFACE('',#6093,0.3);
#5193=CYLINDRICAL_SURFACE('',#6098,0.3);
#5194=CYLINDRICAL_SURFACE('',#6099,0.3);
#5195=CYLINDRICAL_SURFACE('',#6108,0.3);
#5196=CYLINDRICAL_SURFACE('',#6109,0.3);
#5197=CYLINDRICAL_SURFACE('',#6110,0.3);
#5198=CYLINDRICAL_SURFACE('',#6111,0.3);
#5199=CYLINDRICAL_SURFACE('',#6112,0.3);
#5200=CYLINDRICAL_SURFACE('',#6113,0.3);
#5201=CYLINDRICAL_SURFACE('',#6114,0.3);
#5202=CYLINDRICAL_SURFACE('',#6115,0.3);
#5203=CYLINDRICAL_SURFACE('',#6116,0.3);
#5204=CYLINDRICAL_SURFACE('',#6117,0.3);
#5205=CYLINDRICAL_SURFACE('',#6118,0.3);
#5206=CYLINDRICAL_SURFACE('',#6119,0.3);
#5207=CYLINDRICAL_SURFACE('',#6120,0.3);
#5208=CYLINDRICAL_SURFACE('',#6121,0.3);
#5209=CYLINDRICAL_SURFACE('',#6122,0.3);
#5210=CYLINDRICAL_SURFACE('',#6123,0.3);
#5211=CYLINDRICAL_SURFACE('',#6124,0.3);
#5212=CYLINDRICAL_SURFACE('',#6125,0.3);
#5213=CYLINDRICAL_SURFACE('',#6126,0.3);
#5214=CYLINDRICAL_SURFACE('',#6127,0.3);
#5215=CYLINDRICAL_SURFACE('',#6128,0.3);
#5216=CYLINDRICAL_SURFACE('',#6129,0.3);
#5217=CYLINDRICAL_SURFACE('',#6130,0.3);
#5218=CYLINDRICAL_SURFACE('',#6132,0.3);
#5219=CYLINDRICAL_SURFACE('',#6133,0.3);
#5220=CYLINDRICAL_SURFACE('',#6135,0.3);
#5221=CYLINDRICAL_SURFACE('',#6136,0.3);
#5222=CYLINDRICAL_SURFACE('',#6138,0.3);
#5223=CYLINDRICAL_SURFACE('',#6182,4.);
#5224=CYLINDRICAL_SURFACE('',#6189,5.);
#5225=CYLINDRICAL_SURFACE('',#6207,4.);
#5226=CYLINDRICAL_SURFACE('',#6214,5.);
#5227=CYLINDRICAL_SURFACE('',#6231,1.99999999999999);
#5228=CYLINDRICAL_SURFACE('',#6236,1.99999999999999);
#5229=CYLINDRICAL_SURFACE('',#6245,1.99999999999999);
#5230=CYLINDRICAL_SURFACE('',#6251,1.99999999999999);
#5231=CYLINDRICAL_SURFACE('',#6265,0.3);
#5232=CYLINDRICAL_SURFACE('',#6270,0.3);
#5233=CYLINDRICAL_SURFACE('',#6275,0.3);
#5234=CYLINDRICAL_SURFACE('',#6276,0.3);
#5235=CYLINDRICAL_SURFACE('',#6281,0.3);
#5236=CYLINDRICAL_SURFACE('',#6295,0.3);
#5237=CYLINDRICAL_SURFACE('',#6310,0.3);
#5238=CYLINDRICAL_SURFACE('',#6320,0.3);
#5239=CYLINDRICAL_SURFACE('',#6325,0.3);
#5240=CYLINDRICAL_SURFACE('',#6330,0.3);
#5241=CYLINDRICAL_SURFACE('',#6335,0.3);
#5242=CYLINDRICAL_SURFACE('',#6336,0.3);
#5243=CYLINDRICAL_SURFACE('',#6345,0.3);
#5244=CYLINDRICAL_SURFACE('',#6350,0.3);
#5245=CYLINDRICAL_SURFACE('',#6351,0.3);
#5246=CYLINDRICAL_SURFACE('',#6352,0.3);
#5247=CYLINDRICAL_SURFACE('',#6353,0.3);
#5248=CYLINDRICAL_SURFACE('',#6354,0.3);
#5249=CYLINDRICAL_SURFACE('',#6367,0.3);
#5250=CYLINDRICAL_SURFACE('',#6372,0.3);
#5251=CYLINDRICAL_SURFACE('',#6373,0.3);
#5252=CYLINDRICAL_SURFACE('',#6374,0.3);
#5253=CYLINDRICAL_SURFACE('',#6375,0.3);
#5254=CYLINDRICAL_SURFACE('',#6376,0.3);
#5255=CYLINDRICAL_SURFACE('',#6377,0.3);
#5256=CYLINDRICAL_SURFACE('',#6381,0.3);
#5257=CYLINDRICAL_SURFACE('',#6391,0.3);
#5258=CYLINDRICAL_SURFACE('',#6392,0.3);
#5259=CYLINDRICAL_SURFACE('',#6393,0.3);
#5260=CYLINDRICAL_SURFACE('',#6394,0.3);
#5261=CYLINDRICAL_SURFACE('',#6395,0.3);
#5262=CYLINDRICAL_SURFACE('',#6396,0.3);
#5263=CYLINDRICAL_SURFACE('',#6397,0.3);
#5264=CYLINDRICAL_SURFACE('',#6398,0.3);
#5265=CYLINDRICAL_SURFACE('',#6399,0.3);
#5266=CYLINDRICAL_SURFACE('',#6400,0.3);
#5267=CYLINDRICAL_SURFACE('',#6401,0.3);
#5268=CYLINDRICAL_SURFACE('',#6402,0.3);
#5269=CYLINDRICAL_SURFACE('',#6403,0.3);
#5270=CYLINDRICAL_SURFACE('',#6404,0.3);
#5271=CYLINDRICAL_SURFACE('',#6406,4.);
#5272=CYLINDRICAL_SURFACE('',#6407,4.);
#5273=CYLINDRICAL_SURFACE('',#6424,4.925);
#5274=CYLINDRICAL_SURFACE('',#6435,4.);
#5275=CYLINDRICAL_SURFACE('',#6442,5.);
#5276=CYLINDRICAL_SURFACE('',#6455,4.);
#5277=CYLINDRICAL_SURFACE('',#6461,4.);
#5278=CYLINDRICAL_SURFACE('',#6472,4.);
#5279=CYLINDRICAL_SURFACE('',#6479,5.);
#5280=CYLINDRICAL_SURFACE('',#6496,1.99999999999999);
#5281=CYLINDRICAL_SURFACE('',#6501,1.99999999999999);
#5282=CYLINDRICAL_SURFACE('',#6510,1.99999999999999);
#5283=CYLINDRICAL_SURFACE('',#6516,1.99999999999999);
#5284=CYLINDRICAL_SURFACE('',#6530,0.3);
#5285=CYLINDRICAL_SURFACE('',#6535,0.3);
#5286=CYLINDRICAL_SURFACE('',#6540,0.3);
#5287=CYLINDRICAL_SURFACE('',#6541,0.3);
#5288=CYLINDRICAL_SURFACE('',#6546,0.3);
#5289=CYLINDRICAL_SURFACE('',#6560,0.3);
#5290=CYLINDRICAL_SURFACE('',#6575,0.3);
#5291=CYLINDRICAL_SURFACE('',#6585,0.3);
#5292=CYLINDRICAL_SURFACE('',#6590,0.3);
#5293=CYLINDRICAL_SURFACE('',#6595,0.3);
#5294=CYLINDRICAL_SURFACE('',#6600,0.3);
#5295=CYLINDRICAL_SURFACE('',#6601,0.3);
#5296=CYLINDRICAL_SURFACE('',#6610,0.3);
#5297=CYLINDRICAL_SURFACE('',#6615,0.3);
#5298=CYLINDRICAL_SURFACE('',#6616,0.3);
#5299=CYLINDRICAL_SURFACE('',#6617,0.3);
#5300=CYLINDRICAL_SURFACE('',#6618,0.3);
#5301=CYLINDRICAL_SURFACE('',#6619,0.3);
#5302=CYLINDRICAL_SURFACE('',#6632,0.3);
#5303=CYLINDRICAL_SURFACE('',#6637,0.3);
#5304=CYLINDRICAL_SURFACE('',#6638,0.3);
#5305=CYLINDRICAL_SURFACE('',#6639,0.3);
#5306=CYLINDRICAL_SURFACE('',#6640,0.3);
#5307=CYLINDRICAL_SURFACE('',#6641,0.3);
#5308=CYLINDRICAL_SURFACE('',#6642,0.3);
#5309=CYLINDRICAL_SURFACE('',#6646,0.3);
#5310=CYLINDRICAL_SURFACE('',#6656,0.3);
#5311=CYLINDRICAL_SURFACE('',#6657,0.3);
#5312=CYLINDRICAL_SURFACE('',#6658,0.3);
#5313=CYLINDRICAL_SURFACE('',#6659,0.3);
#5314=CYLINDRICAL_SURFACE('',#6660,0.3);
#5315=CYLINDRICAL_SURFACE('',#6661,0.3);
#5316=CYLINDRICAL_SURFACE('',#6662,0.3);
#5317=CYLINDRICAL_SURFACE('',#6663,0.3);
#5318=CYLINDRICAL_SURFACE('',#6664,0.3);
#5319=CYLINDRICAL_SURFACE('',#6665,0.3);
#5320=CYLINDRICAL_SURFACE('',#6666,0.3);
#5321=CYLINDRICAL_SURFACE('',#6667,0.3);
#5322=CYLINDRICAL_SURFACE('',#6668,0.3);
#5323=CYLINDRICAL_SURFACE('',#6669,0.3);
#5324=CYLINDRICAL_SURFACE('',#6671,4.);
#5325=CYLINDRICAL_SURFACE('',#6672,4.);
#5326=ADVANCED_FACE('',(#383),#5152,.F.);
#5327=ADVANCED_FACE('',(#384),#294,.T.);
#5328=ADVANCED_FACE('',(#385,#247),#295,.T.);
#5329=ADVANCED_FACE('',(#386),#296,.T.);
#5330=ADVANCED_FACE('',(#387,#248),#297,.T.);
#5331=ADVANCED_FACE('',(#388),#298,.T.);
#5332=ADVANCED_FACE('',(#389),#179,.T.);
#5333=ADVANCED_FACE('',(#390,#249,#250),#299,.T.);
#5334=ADVANCED_FACE('',(#391),#5153,.F.);
#5335=ADVANCED_FACE('',(#392),#180,.T.);
#5336=ADVANCED_FACE('',(#393),#5154,.F.);
#5337=ADVANCED_FACE('',(#394),#181,.T.);
#5338=ADVANCED_FACE('',(#395,#251,#252),#300,.T.);
#5339=ADVANCED_FACE('',(#396),#182,.T.);
#5340=ADVANCED_FACE('',(#397),#183,.T.);
#5341=ADVANCED_FACE('',(#398,#253,#254,#255,#256,#257,#258,#259,#260,#261,
#262,#263,#264,#265,#266,#267,#268),#301,.T.);
#5342=ADVANCED_FACE('',(#399),#5155,.F.);
#5343=ADVANCED_FACE('',(#400),#184,.T.);
#5344=ADVANCED_FACE('',(#401),#5156,.F.);
#5345=ADVANCED_FACE('',(#402),#185,.T.);
#5346=ADVANCED_FACE('',(#403),#5157,.F.);
#5347=ADVANCED_FACE('',(#404),#186,.T.);
#5348=ADVANCED_FACE('',(#405),#5158,.F.);
#5349=ADVANCED_FACE('',(#406),#187,.T.);
#5350=ADVANCED_FACE('',(#407),#5159,.F.);
#5351=ADVANCED_FACE('',(#408),#188,.T.);
#5352=ADVANCED_FACE('',(#409),#5160,.F.);
#5353=ADVANCED_FACE('',(#410),#189,.T.);
#5354=ADVANCED_FACE('',(#411),#5161,.F.);
#5355=ADVANCED_FACE('',(#412),#190,.T.);
#5356=ADVANCED_FACE('',(#413),#5162,.F.);
#5357=ADVANCED_FACE('',(#414),#191,.T.);
#5358=ADVANCED_FACE('',(#415),#5163,.F.);
#5359=ADVANCED_FACE('',(#416),#192,.T.);
#5360=ADVANCED_FACE('',(#417),#5164,.F.);
#5361=ADVANCED_FACE('',(#418),#193,.T.);
#5362=ADVANCED_FACE('',(#419),#5165,.F.);
#5363=ADVANCED_FACE('',(#420),#194,.T.);
#5364=ADVANCED_FACE('',(#421),#5166,.F.);
#5365=ADVANCED_FACE('',(#422),#195,.T.);
#5366=ADVANCED_FACE('',(#423),#5167,.F.);
#5367=ADVANCED_FACE('',(#424),#196,.T.);
#5368=ADVANCED_FACE('',(#425),#5168,.F.);
#5369=ADVANCED_FACE('',(#426),#197,.T.);
#5370=ADVANCED_FACE('',(#427),#5169,.F.);
#5371=ADVANCED_FACE('',(#428),#198,.T.);
#5372=ADVANCED_FACE('',(#429),#5170,.F.);
#5373=ADVANCED_FACE('',(#430),#5171,.T.);
#5374=ADVANCED_FACE('',(#431),#5172,.T.);
#5375=ADVANCED_FACE('',(#432),#5173,.T.);
#5376=ADVANCED_FACE('',(#433),#5174,.T.);
#5377=ADVANCED_FACE('',(#434),#5175,.T.);
#5378=ADVANCED_FACE('',(#435),#5176,.T.);
#5379=ADVANCED_FACE('',(#436),#5177,.T.);
#5380=ADVANCED_FACE('',(#437),#5178,.T.);
#5381=ADVANCED_FACE('',(#438),#107,.T.);
#5382=ADVANCED_FACE('',(#439),#108,.T.);
#5383=ADVANCED_FACE('',(#440),#5179,.T.);
#5384=ADVANCED_FACE('',(#441),#5180,.T.);
#5385=ADVANCED_FACE('',(#442),#109,.T.);
#5386=ADVANCED_FACE('',(#443),#5181,.T.);
#5387=ADVANCED_FACE('',(#444),#199,.T.);
#5388=ADVANCED_FACE('',(#445),#110,.T.);
#5389=ADVANCED_FACE('',(#446),#5182,.T.);
#5390=ADVANCED_FACE('',(#447),#5183,.T.);
#5391=ADVANCED_FACE('',(#448),#200,.T.);
#5392=ADVANCED_FACE('',(#449),#5184,.T.);
#5393=ADVANCED_FACE('',(#450),#201,.T.);
#5394=ADVANCED_FACE('',(#451),#111,.T.);
#5395=ADVANCED_FACE('',(#452),#202,.T.);
#5396=ADVANCED_FACE('',(#453),#112,.T.);
#5397=ADVANCED_FACE('',(#454),#5185,.T.);
#5398=ADVANCED_FACE('',(#455),#5186,.T.);
#5399=ADVANCED_FACE('',(#456),#113,.T.);
#5400=ADVANCED_FACE('',(#457),#203,.T.);
#5401=ADVANCED_FACE('',(#458),#114,.T.);
#5402=ADVANCED_FACE('',(#459),#5187,.T.);
#5403=ADVANCED_FACE('',(#460),#204,.T.);
#5404=ADVANCED_FACE('',(#461),#5188,.T.);
#5405=ADVANCED_FACE('',(#462),#205,.T.);
#5406=ADVANCED_FACE('',(#463),#5189,.T.);
#5407=ADVANCED_FACE('',(#464),#115,.T.);
#5408=ADVANCED_FACE('',(#465),#206,.T.);
#5409=ADVANCED_FACE('',(#466),#116,.T.);
#5410=ADVANCED_FACE('',(#467),#5190,.T.);
#5411=ADVANCED_FACE('',(#468),#5191,.T.);
#5412=ADVANCED_FACE('',(#469),#117,.T.);
#5413=ADVANCED_FACE('',(#470),#118,.T.);
#5414=ADVANCED_FACE('',(#471),#119,.T.);
#5415=ADVANCED_FACE('',(#472),#5192,.T.);
#5416=ADVANCED_FACE('',(#473),#120,.T.);
#5417=ADVANCED_FACE('',(#474),#5193,.T.);
#5418=ADVANCED_FACE('',(#475),#5194,.T.);
#5419=ADVANCED_FACE('',(#476),#121,.T.);
#5420=ADVANCED_FACE('',(#477),#122,.T.);
#5421=ADVANCED_FACE('',(#478),#5195,.T.);
#5422=ADVANCED_FACE('',(#479),#5196,.T.);
#5423=ADVANCED_FACE('',(#480),#5197,.T.);
#5424=ADVANCED_FACE('',(#481),#5198,.T.);
#5425=ADVANCED_FACE('',(#482),#5199,.T.);
#5426=ADVANCED_FACE('',(#483),#5200,.T.);
#5427=ADVANCED_FACE('',(#484),#5201,.T.);
#5428=ADVANCED_FACE('',(#485),#5202,.T.);
#5429=ADVANCED_FACE('',(#486),#5203,.T.);
#5430=ADVANCED_FACE('',(#487),#5204,.F.);
#5431=ADVANCED_FACE('',(#488),#5205,.T.);
#5432=ADVANCED_FACE('',(#489),#5206,.F.);
#5433=ADVANCED_FACE('',(#490),#5207,.T.);
#5434=ADVANCED_FACE('',(#491),#5208,.T.);
#5435=ADVANCED_FACE('',(#492),#5209,.T.);
#5436=ADVANCED_FACE('',(#493),#5210,.T.);
#5437=ADVANCED_FACE('',(#494),#5211,.F.);
#5438=ADVANCED_FACE('',(#495),#5212,.T.);
#5439=ADVANCED_FACE('',(#496),#5213,.T.);
#5440=ADVANCED_FACE('',(#497),#5214,.F.);
#5441=ADVANCED_FACE('',(#498),#5215,.T.);
#5442=ADVANCED_FACE('',(#499),#5216,.T.);
#5443=ADVANCED_FACE('',(#500),#5217,.T.);
#5444=ADVANCED_FACE('',(#501),#5218,.T.);
#5445=ADVANCED_FACE('',(#502),#5219,.T.);
#5446=ADVANCED_FACE('',(#503),#5220,.T.);
#5447=ADVANCED_FACE('',(#504),#5221,.T.);
#5448=ADVANCED_FACE('',(#505),#5222,.T.);
#5449=ADVANCED_FACE('',(#506),#302,.T.);
#5450=ADVANCED_FACE('',(#507),#303,.T.);
#5451=ADVANCED_FACE('',(#508),#304,.T.);
#5452=ADVANCED_FACE('',(#509,#269),#305,.T.);
#5453=ADVANCED_FACE('',(#510),#306,.F.);
#5454=ADVANCED_FACE('',(#511),#307,.F.);
#5455=ADVANCED_FACE('',(#512),#308,.F.);
#5456=ADVANCED_FACE('',(#513),#309,.F.);
#5457=ADVANCED_FACE('',(#514),#310,.T.);
#5458=ADVANCED_FACE('',(#515),#311,.F.);
#5459=ADVANCED_FACE('',(#516),#312,.T.);
#5460=ADVANCED_FACE('',(#517),#313,.T.);
#5461=ADVANCED_FACE('',(#518),#314,.F.);
#5462=ADVANCED_FACE('',(#519),#315,.F.);
#5463=ADVANCED_FACE('',(#520),#316,.T.);
#5464=ADVANCED_FACE('',(#521),#317,.T.);
#5465=ADVANCED_FACE('',(#522),#318,.T.);
#5466=ADVANCED_FACE('',(#523),#319,.T.);
#5467=ADVANCED_FACE('',(#524),#320,.T.);
#5468=ADVANCED_FACE('',(#525),#321,.T.);
#5469=ADVANCED_FACE('',(#526),#322,.T.);
#5470=ADVANCED_FACE('',(#527),#323,.T.);
#5471=ADVANCED_FACE('',(#528),#324,.T.);
#5472=ADVANCED_FACE('',(#529),#325,.T.);
#5473=ADVANCED_FACE('',(#530),#326,.T.);
#5474=ADVANCED_FACE('',(#531),#327,.T.);
#5475=ADVANCED_FACE('',(#532),#328,.T.);
#5476=ADVANCED_FACE('',(#533),#329,.T.);
#5477=ADVANCED_FACE('',(#534),#330,.T.);
#5478=ADVANCED_FACE('',(#535),#331,.T.);
#5479=ADVANCED_FACE('',(#536),#332,.T.);
#5480=ADVANCED_FACE('',(#537),#333,.T.);
#5481=ADVANCED_FACE('',(#538),#334,.T.);
#5482=ADVANCED_FACE('',(#539),#335,.T.);
#5483=ADVANCED_FACE('',(#540),#336,.T.);
#5484=ADVANCED_FACE('',(#541),#207,.T.);
#5485=ADVANCED_FACE('',(#542,#270),#337,.T.);
#5486=ADVANCED_FACE('',(#543),#5223,.F.);
#5487=ADVANCED_FACE('',(#544),#208,.T.);
#5488=ADVANCED_FACE('',(#545),#5224,.T.);
#5489=ADVANCED_FACE('',(#546),#209,.T.);
#5490=ADVANCED_FACE('',(#547,#271),#338,.F.);
#5491=ADVANCED_FACE('',(#548),#210,.T.);
#5492=ADVANCED_FACE('',(#549),#211,.T.);
#5493=ADVANCED_FACE('',(#550,#272),#339,.F.);
#5494=ADVANCED_FACE('',(#551),#5225,.F.);
#5495=ADVANCED_FACE('',(#552),#212,.T.);
#5496=ADVANCED_FACE('',(#553),#5226,.T.);
#5497=ADVANCED_FACE('',(#554),#213,.T.);
#5498=ADVANCED_FACE('',(#555,#273),#340,.T.);
#5499=ADVANCED_FACE('',(#556),#214,.T.);
#5500=ADVANCED_FACE('',(#557),#215,.T.);
#5501=ADVANCED_FACE('',(#558,#274,#275),#341,.F.);
#5502=ADVANCED_FACE('',(#559),#5227,.F.);
#5503=ADVANCED_FACE('',(#560),#216,.T.);
#5504=ADVANCED_FACE('',(#561),#5228,.F.);
#5505=ADVANCED_FACE('',(#562),#217,.T.);
#5506=ADVANCED_FACE('',(#563,#276,#277),#342,.T.);
#5507=ADVANCED_FACE('',(#564),#5229,.F.);
#5508=ADVANCED_FACE('',(#565),#218,.T.);
#5509=ADVANCED_FACE('',(#566),#5230,.F.);
#5510=ADVANCED_FACE('',(#567),#123,.T.);
#5511=ADVANCED_FACE('',(#568),#124,.T.);
#5512=ADVANCED_FACE('',(#569),#125,.T.);
#5513=ADVANCED_FACE('',(#570),#5231,.T.);
#5514=ADVANCED_FACE('',(#571),#126,.T.);
#5515=ADVANCED_FACE('',(#572),#5232,.T.);
#5516=ADVANCED_FACE('',(#573),#127,.T.);
#5517=ADVANCED_FACE('',(#574),#5233,.T.);
#5518=ADVANCED_FACE('',(#575),#5234,.T.);
#5519=ADVANCED_FACE('',(#576),#128,.T.);
#5520=ADVANCED_FACE('',(#577),#5235,.T.);
#5521=ADVANCED_FACE('',(#578),#129,.T.);
#5522=ADVANCED_FACE('',(#579),#219,.T.);
#5523=ADVANCED_FACE('',(#580),#130,.T.);
#5524=ADVANCED_FACE('',(#581),#5236,.T.);
#5525=ADVANCED_FACE('',(#582),#220,.T.);
#5526=ADVANCED_FACE('',(#583),#221,.T.);
#5527=ADVANCED_FACE('',(#584),#131,.T.);
#5528=ADVANCED_FACE('',(#585),#5237,.T.);
#5529=ADVANCED_FACE('',(#586),#222,.T.);
#5530=ADVANCED_FACE('',(#587),#132,.T.);
#5531=ADVANCED_FACE('',(#588),#5238,.T.);
#5532=ADVANCED_FACE('',(#589),#133,.T.);
#5533=ADVANCED_FACE('',(#590),#5239,.T.);
#5534=ADVANCED_FACE('',(#591),#134,.T.);
#5535=ADVANCED_FACE('',(#592),#5240,.T.);
#5536=ADVANCED_FACE('',(#593),#135,.T.);
#5537=ADVANCED_FACE('',(#594),#5241,.T.);
#5538=ADVANCED_FACE('',(#595),#5242,.T.);
#5539=ADVANCED_FACE('',(#596),#136,.T.);
#5540=ADVANCED_FACE('',(#597),#137,.T.);
#5541=ADVANCED_FACE('',(#598),#5243,.T.);
#5542=ADVANCED_FACE('',(#599),#138,.T.);
#5543=ADVANCED_FACE('',(#600),#5244,.T.);
#5544=ADVANCED_FACE('',(#601),#5245,.T.);
#5545=ADVANCED_FACE('',(#602),#5246,.T.);
#5546=ADVANCED_FACE('',(#603),#5247,.T.);
#5547=ADVANCED_FACE('',(#604),#5248,.T.);
#5548=ADVANCED_FACE('',(#605),#139,.T.);
#5549=ADVANCED_FACE('',(#606),#140,.T.);
#5550=ADVANCED_FACE('',(#607),#141,.T.);
#5551=ADVANCED_FACE('',(#608),#5249,.T.);
#5552=ADVANCED_FACE('',(#609),#142,.T.);
#5553=ADVANCED_FACE('',(#610),#5250,.T.);
#5554=ADVANCED_FACE('',(#611),#5251,.T.);
#5555=ADVANCED_FACE('',(#612),#5252,.T.);
#5556=ADVANCED_FACE('',(#613),#5253,.T.);
#5557=ADVANCED_FACE('',(#614),#5254,.T.);
#5558=ADVANCED_FACE('',(#615),#5255,.T.);
#5559=ADVANCED_FACE('',(#616),#223,.T.);
#5560=ADVANCED_FACE('',(#617),#5256,.T.);
#5561=ADVANCED_FACE('',(#618),#224,.T.);
#5562=ADVANCED_FACE('',(#619),#225,.T.);
#5563=ADVANCED_FACE('',(#620),#226,.T.);
#5564=ADVANCED_FACE('',(#621),#5257,.T.);
#5565=ADVANCED_FACE('',(#622),#5258,.T.);
#5566=ADVANCED_FACE('',(#623),#5259,.T.);
#5567=ADVANCED_FACE('',(#624),#5260,.T.);
#5568=ADVANCED_FACE('',(#625),#5261,.T.);
#5569=ADVANCED_FACE('',(#626),#5262,.F.);
#5570=ADVANCED_FACE('',(#627),#5263,.T.);
#5571=ADVANCED_FACE('',(#628),#5264,.F.);
#5572=ADVANCED_FACE('',(#629),#5265,.T.);
#5573=ADVANCED_FACE('',(#630),#5266,.T.);
#5574=ADVANCED_FACE('',(#631),#5267,.T.);
#5575=ADVANCED_FACE('',(#632),#5268,.T.);
#5576=ADVANCED_FACE('',(#633),#5269,.T.);
#5577=ADVANCED_FACE('',(#634),#5270,.T.);
#5578=ADVANCED_FACE('',(#635),#343,.F.);
#5579=ADVANCED_FACE('',(#636),#5271,.F.);
#5580=ADVANCED_FACE('',(#637),#5272,.F.);
#5581=ADVANCED_FACE('',(#638),#344,.T.);
#5582=ADVANCED_FACE('',(#639,#278,#279,#280,#281),#345,.F.);
#5583=ADVANCED_FACE('',(#640),#346,.F.);
#5584=ADVANCED_FACE('',(#641),#347,.T.);
#5585=ADVANCED_FACE('',(#642),#348,.F.);
#5586=ADVANCED_FACE('',(#643),#349,.F.);
#5587=ADVANCED_FACE('',(#644),#350,.F.);
#5588=ADVANCED_FACE('',(#645),#351,.F.);
#5589=ADVANCED_FACE('',(#646),#352,.F.);
#5590=ADVANCED_FACE('',(#647),#353,.F.);
#5591=ADVANCED_FACE('',(#648),#354,.F.);
#5592=ADVANCED_FACE('',(#649),#355,.F.);
#5593=ADVANCED_FACE('',(#650),#356,.T.);
#5594=ADVANCED_FACE('',(#651),#357,.F.);
#5595=ADVANCED_FACE('',(#652),#5273,.T.);
#5596=ADVANCED_FACE('',(#653),#358,.T.);
#5597=ADVANCED_FACE('',(#654),#227,.T.);
#5598=ADVANCED_FACE('',(#655,#282),#359,.T.);
#5599=ADVANCED_FACE('',(#656),#5274,.F.);
#5600=ADVANCED_FACE('',(#657),#228,.T.);
#5601=ADVANCED_FACE('',(#658),#5275,.T.);
#5602=ADVANCED_FACE('',(#659),#229,.T.);
#5603=ADVANCED_FACE('',(#660,#283),#360,.F.);
#5604=ADVANCED_FACE('',(#661),#230,.T.);
#5605=ADVANCED_FACE('',(#662),#361,.F.);
#5606=ADVANCED_FACE('',(#663),#5276,.T.);
#5607=ADVANCED_FACE('',(#664),#362,.T.);
#5608=ADVANCED_FACE('',(#665),#363,.T.);
#5609=ADVANCED_FACE('',(#666),#5277,.T.);
#5610=ADVANCED_FACE('',(#667),#364,.F.);
#5611=ADVANCED_FACE('',(#668),#231,.T.);
#5612=ADVANCED_FACE('',(#669,#284),#365,.F.);
#5613=ADVANCED_FACE('',(#670),#5278,.F.);
#5614=ADVANCED_FACE('',(#671),#232,.T.);
#5615=ADVANCED_FACE('',(#672),#5279,.T.);
#5616=ADVANCED_FACE('',(#673),#233,.T.);
#5617=ADVANCED_FACE('',(#674,#285),#366,.T.);
#5618=ADVANCED_FACE('',(#675),#234,.T.);
#5619=ADVANCED_FACE('',(#676),#235,.T.);
#5620=ADVANCED_FACE('',(#677,#286,#287),#367,.T.);
#5621=ADVANCED_FACE('',(#678),#5280,.F.);
#5622=ADVANCED_FACE('',(#679),#236,.T.);
#5623=ADVANCED_FACE('',(#680),#5281,.F.);
#5624=ADVANCED_FACE('',(#681),#237,.T.);
#5625=ADVANCED_FACE('',(#682,#288,#289),#368,.F.);
#5626=ADVANCED_FACE('',(#683),#5282,.F.);
#5627=ADVANCED_FACE('',(#684),#238,.T.);
#5628=ADVANCED_FACE('',(#685),#5283,.F.);
#5629=ADVANCED_FACE('',(#686),#143,.T.);
#5630=ADVANCED_FACE('',(#687),#144,.T.);
#5631=ADVANCED_FACE('',(#688),#145,.T.);
#5632=ADVANCED_FACE('',(#689),#5284,.T.);
#5633=ADVANCED_FACE('',(#690),#146,.T.);
#5634=ADVANCED_FACE('',(#691),#5285,.T.);
#5635=ADVANCED_FACE('',(#692),#147,.T.);
#5636=ADVANCED_FACE('',(#693),#5286,.T.);
#5637=ADVANCED_FACE('',(#694),#5287,.T.);
#5638=ADVANCED_FACE('',(#695),#148,.T.);
#5639=ADVANCED_FACE('',(#696),#5288,.T.);
#5640=ADVANCED_FACE('',(#697),#149,.T.);
#5641=ADVANCED_FACE('',(#698),#239,.T.);
#5642=ADVANCED_FACE('',(#699),#150,.T.);
#5643=ADVANCED_FACE('',(#700),#5289,.T.);
#5644=ADVANCED_FACE('',(#701),#240,.T.);
#5645=ADVANCED_FACE('',(#702),#241,.T.);
#5646=ADVANCED_FACE('',(#703),#151,.T.);
#5647=ADVANCED_FACE('',(#704),#5290,.T.);
#5648=ADVANCED_FACE('',(#705),#242,.T.);
#5649=ADVANCED_FACE('',(#706),#152,.T.);
#5650=ADVANCED_FACE('',(#707),#5291,.T.);
#5651=ADVANCED_FACE('',(#708),#153,.T.);
#5652=ADVANCED_FACE('',(#709),#5292,.T.);
#5653=ADVANCED_FACE('',(#710),#154,.T.);
#5654=ADVANCED_FACE('',(#711),#5293,.T.);
#5655=ADVANCED_FACE('',(#712),#155,.T.);
#5656=ADVANCED_FACE('',(#713),#5294,.T.);
#5657=ADVANCED_FACE('',(#714),#5295,.T.);
#5658=ADVANCED_FACE('',(#715),#156,.T.);
#5659=ADVANCED_FACE('',(#716),#157,.T.);
#5660=ADVANCED_FACE('',(#717),#5296,.T.);
#5661=ADVANCED_FACE('',(#718),#158,.T.);
#5662=ADVANCED_FACE('',(#719),#5297,.T.);
#5663=ADVANCED_FACE('',(#720),#5298,.T.);
#5664=ADVANCED_FACE('',(#721),#5299,.T.);
#5665=ADVANCED_FACE('',(#722),#5300,.T.);
#5666=ADVANCED_FACE('',(#723),#5301,.T.);
#5667=ADVANCED_FACE('',(#724),#159,.T.);
#5668=ADVANCED_FACE('',(#725),#160,.T.);
#5669=ADVANCED_FACE('',(#726),#161,.T.);
#5670=ADVANCED_FACE('',(#727),#5302,.T.);
#5671=ADVANCED_FACE('',(#728),#162,.T.);
#5672=ADVANCED_FACE('',(#729),#5303,.T.);
#5673=ADVANCED_FACE('',(#730),#5304,.T.);
#5674=ADVANCED_FACE('',(#731),#5305,.T.);
#5675=ADVANCED_FACE('',(#732),#5306,.T.);
#5676=ADVANCED_FACE('',(#733),#5307,.T.);
#5677=ADVANCED_FACE('',(#734),#5308,.T.);
#5678=ADVANCED_FACE('',(#735),#243,.T.);
#5679=ADVANCED_FACE('',(#736),#5309,.T.);
#5680=ADVANCED_FACE('',(#737),#244,.T.);
#5681=ADVANCED_FACE('',(#738),#245,.T.);
#5682=ADVANCED_FACE('',(#739),#246,.T.);
#5683=ADVANCED_FACE('',(#740),#5310,.T.);
#5684=ADVANCED_FACE('',(#741),#5311,.T.);
#5685=ADVANCED_FACE('',(#742),#5312,.T.);
#5686=ADVANCED_FACE('',(#743),#5313,.T.);
#5687=ADVANCED_FACE('',(#744),#5314,.T.);
#5688=ADVANCED_FACE('',(#745),#5315,.F.);
#5689=ADVANCED_FACE('',(#746),#5316,.T.);
#5690=ADVANCED_FACE('',(#747),#5317,.F.);
#5691=ADVANCED_FACE('',(#748),#5318,.T.);
#5692=ADVANCED_FACE('',(#749),#5319,.T.);
#5693=ADVANCED_FACE('',(#750),#5320,.T.);
#5694=ADVANCED_FACE('',(#751),#5321,.T.);
#5695=ADVANCED_FACE('',(#752),#5322,.T.);
#5696=ADVANCED_FACE('',(#753),#5323,.T.);
#5697=ADVANCED_FACE('',(#754),#369,.T.);
#5698=ADVANCED_FACE('',(#755),#5324,.F.);
#5699=ADVANCED_FACE('',(#756),#5325,.F.);
#5700=ADVANCED_FACE('',(#757),#370,.F.);
#5701=ADVANCED_FACE('',(#758,#290,#291,#292,#293),#371,.T.);
#5702=ADVANCED_FACE('',(#759),#372,.T.);
#5703=ADVANCED_FACE('',(#760),#373,.F.);
#5704=ADVANCED_FACE('',(#761),#374,.T.);
#5705=ADVANCED_FACE('',(#762),#375,.T.);
#5706=ADVANCED_FACE('',(#763),#376,.T.);
#5707=ADVANCED_FACE('',(#764),#377,.T.);
#5708=ADVANCED_FACE('',(#765),#378,.T.);
#5709=ADVANCED_FACE('',(#766),#379,.T.);
#5710=ADVANCED_FACE('',(#767),#380,.T.);
#5711=ADVANCED_FACE('',(#768),#381,.T.);
#5712=ADVANCED_FACE('',(#769),#382,.F.);
#5713=CLOSED_SHELL('',(#5326,#5327,#5328,#5329,#5330,#5331,#5332,#5333,
#5334,#5335,#5336,#5337,#5338,#5339,#5340,#5341,#5342,#5343,#5344,#5345,
#5346,#5347,#5348,#5349,#5350,#5351,#5352,#5353,#5354,#5355,#5356,#5357,
#5358,#5359,#5360,#5361,#5362,#5363,#5364,#5365,#5366,#5367,#5368,#5369,
#5370,#5371,#5372,#5373,#5374,#5375,#5376,#5377,#5378,#5379,#5380,#5381,
#5382,#5383,#5384,#5385,#5386,#5387,#5388,#5389,#5390,#5391,#5392,#5393,
#5394,#5395,#5396,#5397,#5398,#5399,#5400,#5401,#5402,#5403,#5404,#5405,
#5406,#5407,#5408,#5409,#5410,#5411,#5412,#5413,#5414,#5415,#5416,#5417,
#5418,#5419,#5420,#5421,#5422,#5423,#5424,#5425,#5426,#5427,#5428,#5429,
#5430,#5431,#5432,#5433,#5434,#5435,#5436,#5437,#5438,#5439,#5440,#5441,
#5442,#5443,#5444,#5445,#5446,#5447,#5448,#5449,#5450,#5451,#5452,#5453,
#5454,#5455,#5456,#5457,#5458,#5459,#5460,#5461,#5462,#5463,#5464,#5465,
#5466,#5467,#5468,#5469,#5470,#5471,#5472,#5473,#5474,#5475,#5476,#5477,
#5478,#5479,#5480,#5481,#5482,#5483));
#5714=CLOSED_SHELL('',(#5484,#5485,#5486,#5487,#5488,#5489,#5490,#5491));
#5715=CLOSED_SHELL('',(#5492,#5493,#5494,#5495,#5496,#5497,#5498,#5499));
#5716=CLOSED_SHELL('',(#5500,#5501,#5502,#5503,#5504,#5505,#5506,#5507,
#5508,#5509,#5510,#5511,#5512,#5513,#5514,#5515,#5516,#5517,#5518,#5519,
#5520,#5521,#5522,#5523,#5524,#5525,#5526,#5527,#5528,#5529,#5530,#5531,
#5532,#5533,#5534,#5535,#5536,#5537,#5538,#5539,#5540,#5541,#5542,#5543,
#5544,#5545,#5546,#5547,#5548,#5549,#5550,#5551,#5552,#5553,#5554,#5555,
#5556,#5557,#5558,#5559,#5560,#5561,#5562,#5563,#5564,#5565,#5566,#5567,
#5568,#5569,#5570,#5571,#5572,#5573,#5574,#5575,#5576,#5577,#5578,#5579,
#5580,#5581,#5582,#5583,#5584,#5585,#5586,#5587,#5588,#5589,#5590,#5591,
#5592,#5593));
#5717=CLOSED_SHELL('',(#5594,#5595,#5596));
#5718=CLOSED_SHELL('',(#5597,#5598,#5599,#5600,#5601,#5602,#5603,#5604));
#5719=CLOSED_SHELL('',(#5605,#5606,#5607));
#5720=CLOSED_SHELL('',(#5608,#5609,#5610));
#5721=CLOSED_SHELL('',(#5611,#5612,#5613,#5614,#5615,#5616,#5617,#5618));
#5722=CLOSED_SHELL('',(#5619,#5620,#5621,#5622,#5623,#5624,#5625,#5626,
#5627,#5628,#5629,#5630,#5631,#5632,#5633,#5634,#5635,#5636,#5637,#5638,
#5639,#5640,#5641,#5642,#5643,#5644,#5645,#5646,#5647,#5648,#5649,#5650,
#5651,#5652,#5653,#5654,#5655,#5656,#5657,#5658,#5659,#5660,#5661,#5662,
#5663,#5664,#5665,#5666,#5667,#5668,#5669,#5670,#5671,#5672,#5673,#5674,
#5675,#5676,#5677,#5678,#5679,#5680,#5681,#5682,#5683,#5684,#5685,#5686,
#5687,#5688,#5689,#5690,#5691,#5692,#5693,#5694,#5695,#5696,#5697,#5698,
#5699,#5700,#5701,#5702,#5703,#5704,#5705,#5706,#5707,#5708,#5709,#5710,
#5711,#5712));
#5723=DERIVED_UNIT_ELEMENT(#5743,1.);
#5724=DERIVED_UNIT_ELEMENT(#10641,-3.);
#5725=DERIVED_UNIT_ELEMENT(#5743,1.);
#5726=DERIVED_UNIT_ELEMENT(#10641,-3.);
#5727=DERIVED_UNIT_ELEMENT(#5743,1.);
#5728=DERIVED_UNIT_ELEMENT(#10641,-3.);
#5729=DERIVED_UNIT_ELEMENT(#5743,1.);
#5730=DERIVED_UNIT_ELEMENT(#10641,-3.);
#5731=DERIVED_UNIT_ELEMENT(#5743,1.);
#5732=DERIVED_UNIT_ELEMENT(#10641,-3.);
#5733=DERIVED_UNIT_ELEMENT(#5743,1.);
#5734=DERIVED_UNIT_ELEMENT(#10641,-3.);
#5735=DERIVED_UNIT_ELEMENT(#5743,1.);
#5736=DERIVED_UNIT_ELEMENT(#10641,-3.);
#5737=DERIVED_UNIT_ELEMENT(#5743,1.);
#5738=DERIVED_UNIT_ELEMENT(#10641,-3.);
#5739=DERIVED_UNIT_ELEMENT(#5743,1.);
#5740=DERIVED_UNIT_ELEMENT(#10641,-3.);
#5741=DERIVED_UNIT_ELEMENT(#5743,1.);
#5742=DERIVED_UNIT_ELEMENT(#10641,-3.);
#5743=(
MASS_UNIT()
NAMED_UNIT(*)
SI_UNIT(.KILO.,.GRAM.)
);
#5744=DERIVED_UNIT((#5723,#5724));
#5745=DERIVED_UNIT((#5725,#5726));
#5746=DERIVED_UNIT((#5727,#5728));
#5747=DERIVED_UNIT((#5729,#5730));
#5748=DERIVED_UNIT((#5731,#5732));
#5749=DERIVED_UNIT((#5733,#5734));
#5750=DERIVED_UNIT((#5735,#5736));
#5751=DERIVED_UNIT((#5737,#5738));
#5752=DERIVED_UNIT((#5739,#5740));
#5753=DERIVED_UNIT((#5741,#5742));
#5754=MEASURE_REPRESENTATION_ITEM('density measure',
POSITIVE_RATIO_MEASURE(7850.),#5744);
#5755=MEASURE_REPRESENTATION_ITEM('density measure',
POSITIVE_RATIO_MEASURE(7850.),#5745);
#5756=MEASURE_REPRESENTATION_ITEM('density measure',
POSITIVE_RATIO_MEASURE(7850.),#5746);
#5757=MEASURE_REPRESENTATION_ITEM('density measure',
POSITIVE_RATIO_MEASURE(7850.),#5747);
#5758=MEASURE_REPRESENTATION_ITEM('density measure',
POSITIVE_RATIO_MEASURE(7850.),#5748);
#5759=MEASURE_REPRESENTATION_ITEM('density measure',
POSITIVE_RATIO_MEASURE(7850.),#5749);
#5760=MEASURE_REPRESENTATION_ITEM('density measure',
POSITIVE_RATIO_MEASURE(7850.),#5750);
#5761=MEASURE_REPRESENTATION_ITEM('density measure',
POSITIVE_RATIO_MEASURE(7850.),#5751);
#5762=MEASURE_REPRESENTATION_ITEM('density measure',
POSITIVE_RATIO_MEASURE(7850.),#5752);
#5763=MEASURE_REPRESENTATION_ITEM('density measure',
POSITIVE_RATIO_MEASURE(7850.),#5753);
#5764=PROPERTY_DEFINITION_REPRESENTATION(#5814,#5784);
#5765=PROPERTY_DEFINITION_REPRESENTATION(#5815,#5785);
#5766=PROPERTY_DEFINITION_REPRESENTATION(#5816,#5786);
#5767=PROPERTY_DEFINITION_REPRESENTATION(#5817,#5787);
#5768=PROPERTY_DEFINITION_REPRESENTATION(#5818,#5788);
#5769=PROPERTY_DEFINITION_REPRESENTATION(#5819,#5789);
#5770=PROPERTY_DEFINITION_REPRESENTATION(#5820,#5790);
#5771=PROPERTY_DEFINITION_REPRESENTATION(#5821,#5791);
#5772=PROPERTY_DEFINITION_REPRESENTATION(#5822,#5792);
#5773=PROPERTY_DEFINITION_REPRESENTATION(#5823,#5793);
#5774=PROPERTY_DEFINITION_REPRESENTATION(#5824,#5794);
#5775=PROPERTY_DEFINITION_REPRESENTATION(#5825,#5795);
#5776=PROPERTY_DEFINITION_REPRESENTATION(#5826,#5796);
#5777=PROPERTY_DEFINITION_REPRESENTATION(#5827,#5797);
#5778=PROPERTY_DEFINITION_REPRESENTATION(#5828,#5798);
#5779=PROPERTY_DEFINITION_REPRESENTATION(#5829,#5799);
#5780=PROPERTY_DEFINITION_REPRESENTATION(#5830,#5800);
#5781=PROPERTY_DEFINITION_REPRESENTATION(#5831,#5801);
#5782=PROPERTY_DEFINITION_REPRESENTATION(#5832,#5802);
#5783=PROPERTY_DEFINITION_REPRESENTATION(#5833,#5803);
#5784=REPRESENTATION('material name',(#5804),#10629);
#5785=REPRESENTATION('density',(#5754),#10629);
#5786=REPRESENTATION('material name',(#5805),#10630);
#5787=REPRESENTATION('density',(#5755),#10630);
#5788=REPRESENTATION('material name',(#5806),#10631);
#5789=REPRESENTATION('density',(#5756),#10631);
#5790=REPRESENTATION('material name',(#5807),#10632);
#5791=REPRESENTATION('density',(#5757),#10632);
#5792=REPRESENTATION('material name',(#5808),#10633);
#5793=REPRESENTATION('density',(#5758),#10633);
#5794=REPRESENTATION('material name',(#5809),#10634);
#5795=REPRESENTATION('density',(#5759),#10634);
#5796=REPRESENTATION('material name',(#5810),#10635);
#5797=REPRESENTATION('density',(#5760),#10635);
#5798=REPRESENTATION('material name',(#5811),#10636);
#5799=REPRESENTATION('density',(#5761),#10636);
#5800=REPRESENTATION('material name',(#5812),#10637);
#5801=REPRESENTATION('density',(#5762),#10637);
#5802=REPRESENTATION('material name',(#5813),#10638);
#5803=REPRESENTATION('density',(#5763),#10638);
#5804=DESCRIPTIVE_REPRESENTATION_ITEM('Steel','Steel');
#5805=DESCRIPTIVE_REPRESENTATION_ITEM('Steel','Steel');
#5806=DESCRIPTIVE_REPRESENTATION_ITEM('Steel','Steel');
#5807=DESCRIPTIVE_REPRESENTATION_ITEM('Steel','Steel');
#5808=DESCRIPTIVE_REPRESENTATION_ITEM('Steel','Steel');
#5809=DESCRIPTIVE_REPRESENTATION_ITEM('Steel','Steel');
#5810=DESCRIPTIVE_REPRESENTATION_ITEM('Steel','Steel');
#5811=DESCRIPTIVE_REPRESENTATION_ITEM('Steel','Steel');
#5812=DESCRIPTIVE_REPRESENTATION_ITEM('Steel','Steel');
#5813=DESCRIPTIVE_REPRESENTATION_ITEM('Steel','Steel');
#5814=PROPERTY_DEFINITION('material property','material name',#10689);
#5815=PROPERTY_DEFINITION('material property','density of part',#10689);
#5816=PROPERTY_DEFINITION('material property','material name',#10690);
#5817=PROPERTY_DEFINITION('material property','density of part',#10690);
#5818=PROPERTY_DEFINITION('material property','material name',#10691);
#5819=PROPERTY_DEFINITION('material property','density of part',#10691);
#5820=PROPERTY_DEFINITION('material property','material name',#10692);
#5821=PROPERTY_DEFINITION('material property','density of part',#10692);
#5822=PROPERTY_DEFINITION('material property','material name',#10693);
#5823=PROPERTY_DEFINITION('material property','density of part',#10693);
#5824=PROPERTY_DEFINITION('material property','material name',#10694);
#5825=PROPERTY_DEFINITION('material property','density of part',#10694);
#5826=PROPERTY_DEFINITION('material property','material name',#10695);
#5827=PROPERTY_DEFINITION('material property','density of part',#10695);
#5828=PROPERTY_DEFINITION('material property','material name',#10696);
#5829=PROPERTY_DEFINITION('material property','density of part',#10696);
#5830=PROPERTY_DEFINITION('material property','material name',#10697);
#5831=PROPERTY_DEFINITION('material property','density of part',#10697);
#5832=PROPERTY_DEFINITION('material property','material name',#10698);
#5833=PROPERTY_DEFINITION('material property','density of part',#10698);
#5834=AXIS2_PLACEMENT_3D('',#8750,#6696,#6697);
#5835=AXIS2_PLACEMENT_3D('',#8751,#6698,#6699);
#5836=AXIS2_PLACEMENT_3D('',#8752,#6700,#6701);
#5837=AXIS2_PLACEMENT_3D('',#8754,#6702,#6703);
#5838=AXIS2_PLACEMENT_3D('',#8757,#6705,#6706);
#5839=AXIS2_PLACEMENT_3D('',#8758,#6707,#6708);
#5840=AXIS2_PLACEMENT_3D('',#8767,#6713,#6714);
#5841=AXIS2_PLACEMENT_3D('',#8773,#6718,#6719);
#5842=AXIS2_PLACEMENT_3D('',#8779,#6723,#6724);
#5843=AXIS2_PLACEMENT_3D('',#8782,#6727,#6728);
#5844=AXIS2_PLACEMENT_3D('',#8783,#6729,#6730);
#5845=AXIS2_PLACEMENT_3D('',#8785,#6731,#6732);
#5846=AXIS2_PLACEMENT_3D('',#8787,#6733,#6734);
#5847=AXIS2_PLACEMENT_3D('',#8789,#6735,#6736);
#5848=AXIS2_PLACEMENT_3D('',#8790,#6737,#6738);
#5849=AXIS2_PLACEMENT_3D('',#8791,#6739,#6740);
#5850=AXIS2_PLACEMENT_3D('',#8798,#6743,#6744);
#5851=AXIS2_PLACEMENT_3D('',#8804,#6747,#6748);
#5852=AXIS2_PLACEMENT_3D('',#8828,#6760,#6761);
#5853=AXIS2_PLACEMENT_3D('',#8834,#6764,#6765);
#5854=AXIS2_PLACEMENT_3D('',#8841,#6769,#6770);
#5855=AXIS2_PLACEMENT_3D('',#8842,#6771,#6772);
#5856=AXIS2_PLACEMENT_3D('',#8846,#6774,#6775);
#5857=AXIS2_PLACEMENT_3D('',#8847,#6776,#6777);
#5858=AXIS2_PLACEMENT_3D('',#8848,#6778,#6779);
#5859=AXIS2_PLACEMENT_3D('',#8851,#6780,#6781);
#5860=AXIS2_PLACEMENT_3D('',#8852,#6782,#6783);
#5861=AXIS2_PLACEMENT_3D('',#8853,#6784,#6785);
#5862=AXIS2_PLACEMENT_3D('',#8854,#6786,#6787);
#5863=AXIS2_PLACEMENT_3D('',#8858,#6789,#6790);
#5864=AXIS2_PLACEMENT_3D('',#8859,#6791,#6792);
#5865=AXIS2_PLACEMENT_3D('',#8860,#6793,#6794);
#5866=AXIS2_PLACEMENT_3D('',#8862,#6795,#6796);
#5867=AXIS2_PLACEMENT_3D('',#8863,#6797,#6798);
#5868=AXIS2_PLACEMENT_3D('',#8864,#6799,#6800);
#5869=AXIS2_PLACEMENT_3D('',#8867,#6801,#6802);
#5870=AXIS2_PLACEMENT_3D('',#8879,#6808,#6809);
#5871=AXIS2_PLACEMENT_3D('',#8885,#6812,#6813);
#5872=AXIS2_PLACEMENT_3D('',#8909,#6825,#6826);
#5873=AXIS2_PLACEMENT_3D('',#8914,#6829,#6830);
#5874=AXIS2_PLACEMENT_3D('',#8915,#6831,#6832);
#5875=AXIS2_PLACEMENT_3D('',#8916,#6833,#6834);
#5876=AXIS2_PLACEMENT_3D('',#8917,#6835,#6836);
#5877=AXIS2_PLACEMENT_3D('',#8919,#6837,#6838);
#5878=AXIS2_PLACEMENT_3D('',#8921,#6839,#6840);
#5879=AXIS2_PLACEMENT_3D('',#8922,#6841,#6842);
#5880=AXIS2_PLACEMENT_3D('',#8923,#6843,#6844);
#5881=AXIS2_PLACEMENT_3D('',#8933,#6849,#6850);
#5882=AXIS2_PLACEMENT_3D('',#8935,#6851,#6852);
#5883=AXIS2_PLACEMENT_3D('',#8937,#6853,#6854);
#5884=AXIS2_PLACEMENT_3D('',#8939,#6855,#6856);
#5885=AXIS2_PLACEMENT_3D('',#8941,#6857,#6858);
#5886=AXIS2_PLACEMENT_3D('',#8943,#6859,#6860);
#5887=AXIS2_PLACEMENT_3D('',#8945,#6861,#6862);
#5888=AXIS2_PLACEMENT_3D('',#8947,#6863,#6864);
#5889=AXIS2_PLACEMENT_3D('',#8949,#6865,#6866);
#5890=AXIS2_PLACEMENT_3D('',#8951,#6867,#6868);
#5891=AXIS2_PLACEMENT_3D('',#8953,#6869,#6870);
#5892=AXIS2_PLACEMENT_3D('',#8955,#6871,#6872);
#5893=AXIS2_PLACEMENT_3D('',#8957,#6873,#6874);
#5894=AXIS2_PLACEMENT_3D('',#8959,#6875,#6876);
#5895=AXIS2_PLACEMENT_3D('',#8961,#6877,#6878);
#5896=AXIS2_PLACEMENT_3D('',#8962,#6879,#6880);
#5897=AXIS2_PLACEMENT_3D('',#8965,#6882,#6883);
#5898=AXIS2_PLACEMENT_3D('',#8966,#6884,#6885);
#5899=AXIS2_PLACEMENT_3D('',#8968,#6886,#6887);
#5900=AXIS2_PLACEMENT_3D('',#8969,#6888,#6889);
#5901=AXIS2_PLACEMENT_3D('',#8970,#6890,#6891);
#5902=AXIS2_PLACEMENT_3D('',#8973,#6893,#6894);
#5903=AXIS2_PLACEMENT_3D('',#8974,#6895,#6896);
#5904=AXIS2_PLACEMENT_3D('',#8976,#6897,#6898);
#5905=AXIS2_PLACEMENT_3D('',#8977,#6899,#6900);
#5906=AXIS2_PLACEMENT_3D('',#8978,#6901,#6902);
#5907=AXIS2_PLACEMENT_3D('',#8981,#6904,#6905);
#5908=AXIS2_PLACEMENT_3D('',#8982,#6906,#6907);
#5909=AXIS2_PLACEMENT_3D('',#8984,#6908,#6909);
#5910=AXIS2_PLACEMENT_3D('',#8985,#6910,#6911);
#5911=AXIS2_PLACEMENT_3D('',#8986,#6912,#6913);
#5912=AXIS2_PLACEMENT_3D('',#8989,#6915,#6916);
#5913=AXIS2_PLACEMENT_3D('',#8990,#6917,#6918);
#5914=AXIS2_PLACEMENT_3D('',#8992,#6919,#6920);
#5915=AXIS2_PLACEMENT_3D('',#8993,#6921,#6922);
#5916=AXIS2_PLACEMENT_3D('',#8994,#6923,#6924);
#5917=AXIS2_PLACEMENT_3D('',#8997,#6926,#6927);
#5918=AXIS2_PLACEMENT_3D('',#8998,#6928,#6929);
#5919=AXIS2_PLACEMENT_3D('',#9000,#6930,#6931);
#5920=AXIS2_PLACEMENT_3D('',#9001,#6932,#6933);
#5921=AXIS2_PLACEMENT_3D('',#9002,#6934,#6935);
#5922=AXIS2_PLACEMENT_3D('',#9005,#6937,#6938);
#5923=AXIS2_PLACEMENT_3D('',#9006,#6939,#6940);
#5924=AXIS2_PLACEMENT_3D('',#9008,#6941,#6942);
#5925=AXIS2_PLACEMENT_3D('',#9009,#6943,#6944);
#5926=AXIS2_PLACEMENT_3D('',#9010,#6945,#6946);
#5927=AXIS2_PLACEMENT_3D('',#9013,#6948,#6949);
#5928=AXIS2_PLACEMENT_3D('',#9014,#6950,#6951);
#5929=AXIS2_PLACEMENT_3D('',#9016,#6952,#6953);
#5930=AXIS2_PLACEMENT_3D('',#9018,#6954,#6955);
#5931=AXIS2_PLACEMENT_3D('',#9019,#6956,#6957);
#5932=AXIS2_PLACEMENT_3D('',#9020,#6958,#6959);
#5933=AXIS2_PLACEMENT_3D('',#9023,#6961,#6962);
#5934=AXIS2_PLACEMENT_3D('',#9024,#6963,#6964);
#5935=AXIS2_PLACEMENT_3D('',#9026,#6965,#6966);
#5936=AXIS2_PLACEMENT_3D('',#9027,#6967,#6968);
#5937=AXIS2_PLACEMENT_3D('',#9028,#6969,#6970);
#5938=AXIS2_PLACEMENT_3D('',#9031,#6972,#6973);
#5939=AXIS2_PLACEMENT_3D('',#9032,#6974,#6975);
#5940=AXIS2_PLACEMENT_3D('',#9034,#6976,#6977);
#5941=AXIS2_PLACEMENT_3D('',#9036,#6978,#6979);
#5942=AXIS2_PLACEMENT_3D('',#9037,#6980,#6981);
#5943=AXIS2_PLACEMENT_3D('',#9038,#6982,#6983);
#5944=AXIS2_PLACEMENT_3D('',#9041,#6985,#6986);
#5945=AXIS2_PLACEMENT_3D('',#9042,#6987,#6988);
#5946=AXIS2_PLACEMENT_3D('',#9044,#6989,#6990);
#5947=AXIS2_PLACEMENT_3D('',#9045,#6991,#6992);
#5948=AXIS2_PLACEMENT_3D('',#9046,#6993,#6994);
#5949=AXIS2_PLACEMENT_3D('',#9049,#6996,#6997);
#5950=AXIS2_PLACEMENT_3D('',#9050,#6998,#6999);
#5951=AXIS2_PLACEMENT_3D('',#9052,#7000,#7001);
#5952=AXIS2_PLACEMENT_3D('',#9053,#7002,#7003);
#5953=AXIS2_PLACEMENT_3D('',#9054,#7004,#7005);
#5954=AXIS2_PLACEMENT_3D('',#9057,#7007,#7008);
#5955=AXIS2_PLACEMENT_3D('',#9058,#7009,#7010);
#5956=AXIS2_PLACEMENT_3D('',#9060,#7011,#7012);
#5957=AXIS2_PLACEMENT_3D('',#9061,#7013,#7014);
#5958=AXIS2_PLACEMENT_3D('',#9062,#7015,#7016);
#5959=AXIS2_PLACEMENT_3D('',#9065,#7018,#7019);
#5960=AXIS2_PLACEMENT_3D('',#9066,#7020,#7021);
#5961=AXIS2_PLACEMENT_3D('',#9068,#7022,#7023);
#5962=AXIS2_PLACEMENT_3D('',#9069,#7024,#7025);
#5963=AXIS2_PLACEMENT_3D('',#9070,#7026,#7027);
#5964=AXIS2_PLACEMENT_3D('',#9073,#7029,#7030);
#5965=AXIS2_PLACEMENT_3D('',#9074,#7031,#7032);
#5966=AXIS2_PLACEMENT_3D('',#9076,#7033,#7034);
#5967=AXIS2_PLACEMENT_3D('',#9077,#7035,#7036);
#5968=AXIS2_PLACEMENT_3D('',#9078,#7037,#7038);
#5969=AXIS2_PLACEMENT_3D('',#9081,#7040,#7041);
#5970=AXIS2_PLACEMENT_3D('',#9082,#7042,#7043);
#5971=AXIS2_PLACEMENT_3D('',#9084,#7044,#7045);
#5972=AXIS2_PLACEMENT_3D('',#9085,#7046,#7047);
#5973=AXIS2_PLACEMENT_3D('',#9086,#7048,#7049);
#5974=AXIS2_PLACEMENT_3D('',#9089,#7051,#7052);
#5975=AXIS2_PLACEMENT_3D('',#9090,#7053,#7054);
#5976=AXIS2_PLACEMENT_3D('',#9092,#7055,#7056);
#5977=AXIS2_PLACEMENT_3D('',#9095,#7058,#7059);
#5978=AXIS2_PLACEMENT_3D('',#9096,#7060,#7061);
#5979=AXIS2_PLACEMENT_3D('',#9098,#7062,#7063);
#5980=AXIS2_PLACEMENT_3D('',#9101,#7065,#7066);
#5981=AXIS2_PLACEMENT_3D('',#9102,#7067,#7068);
#5982=AXIS2_PLACEMENT_3D('',#9104,#7069,#7070);
#5983=AXIS2_PLACEMENT_3D('',#9106,#7072,#7073);
#5984=AXIS2_PLACEMENT_3D('',#9108,#7074,#7075);
#5985=AXIS2_PLACEMENT_3D('',#9110,#7077,#7078);
#5986=AXIS2_PLACEMENT_3D('',#9112,#7079,#7080);
#5987=AXIS2_PLACEMENT_3D('',#9114,#7082,#7083);
#5988=AXIS2_PLACEMENT_3D('',#9116,#7084,#7085);
#5989=AXIS2_PLACEMENT_3D('',#9118,#7087,#7088);
#5990=AXIS2_PLACEMENT_3D('',#9122,#7090,#7091);
#5991=AXIS2_PLACEMENT_3D('',#9123,#7092,#7093);
#5992=AXIS2_PLACEMENT_3D('',#9124,#7094,#7095);
#5993=AXIS2_PLACEMENT_3D('',#9126,#7096,#7097);
#5994=AXIS2_PLACEMENT_3D('',#9128,#7099,#7100);
#5995=AXIS2_PLACEMENT_3D('',#9130,#7101,#7102);
#5996=AXIS2_PLACEMENT_3D('',#9132,#7103,#7104);
#5997=AXIS2_PLACEMENT_3D('',#9133,#7105,#7106);
#5998=AXIS2_PLACEMENT_3D('',#9134,#7107,#7108);
#5999=AXIS2_PLACEMENT_3D('',#9136,#7109,#7110);
#6000=AXIS2_PLACEMENT_3D('',#9138,#7111,#7112);
#6001=AXIS2_PLACEMENT_3D('',#9139,#7113,#7114);
#6002=AXIS2_PLACEMENT_3D('',#9140,#7115,#7116);
#6003=AXIS2_PLACEMENT_3D('',#9143,#7119,#7120);
#6004=AXIS2_PLACEMENT_3D('',#9145,#7122,#7123);
#6005=AXIS2_PLACEMENT_3D('',#9148,#7124,#7125);
#6006=AXIS2_PLACEMENT_3D('',#9149,#7126,#7127);
#6007=AXIS2_PLACEMENT_3D('',#9150,#7128,#7129);
#6008=AXIS2_PLACEMENT_3D('',#9151,#7130,#7131);
#6009=AXIS2_PLACEMENT_3D('',#9154,#7133,#7134);
#6010=AXIS2_PLACEMENT_3D('',#9155,#7135,#7136);
#6011=AXIS2_PLACEMENT_3D('',#9158,#7137,#7138);
#6012=AXIS2_PLACEMENT_3D('',#9159,#7139,#7140);
#6013=AXIS2_PLACEMENT_3D('',#9160,#7141,#7142);
#6014=AXIS2_PLACEMENT_3D('',#9161,#7143,#7144);
#6015=AXIS2_PLACEMENT_3D('',#9163,#7145,#7146);
#6016=AXIS2_PLACEMENT_3D('',#9165,#7147,#7148);
#6017=AXIS2_PLACEMENT_3D('',#9166,#7149,#7150);
#6018=AXIS2_PLACEMENT_3D('',#9167,#7151,#7152);
#6019=AXIS2_PLACEMENT_3D('',#9170,#7154,#7155);
#6020=AXIS2_PLACEMENT_3D('',#9171,#7156,#7157);
#6021=AXIS2_PLACEMENT_3D('',#9174,#7160,#7161);
#6022=AXIS2_PLACEMENT_3D('',#9177,#7162,#7163);
#6023=AXIS2_PLACEMENT_3D('',#9178,#7164,#7165);
#6024=AXIS2_PLACEMENT_3D('',#9179,#7166,#7167);
#6025=AXIS2_PLACEMENT_3D('',#9180,#7168,#7169);
#6026=AXIS2_PLACEMENT_3D('',#9182,#7171,#7172);
#6027=AXIS2_PLACEMENT_3D('',#9184,#7173,#7174);
#6028=AXIS2_PLACEMENT_3D('',#9186,#7175,#7176);
#6029=AXIS2_PLACEMENT_3D('',#9187,#7177,#7178);
#6030=AXIS2_PLACEMENT_3D('',#9188,#7179,#7180);
#6031=AXIS2_PLACEMENT_3D('',#9190,#7181,#7182);
#6032=AXIS2_PLACEMENT_3D('',#9192,#7183,#7184);
#6033=AXIS2_PLACEMENT_3D('',#9193,#7185,#7186);
#6034=AXIS2_PLACEMENT_3D('',#9194,#7187,#7188);
#6035=AXIS2_PLACEMENT_3D('',#9197,#7189,#7190);
#6036=AXIS2_PLACEMENT_3D('',#9198,#7191,#7192);
#6037=AXIS2_PLACEMENT_3D('',#9199,#7193,#7194);
#6038=AXIS2_PLACEMENT_3D('',#9200,#7195,#7196);
#6039=AXIS2_PLACEMENT_3D('',#9202,#7197,#7198);
#6040=AXIS2_PLACEMENT_3D('',#9204,#7199,#7200);
#6041=AXIS2_PLACEMENT_3D('',#9205,#7201,#7202);
#6042=AXIS2_PLACEMENT_3D('',#9206,#7203,#7204);
#6043=AXIS2_PLACEMENT_3D('',#9209,#7207,#7208);
#6044=AXIS2_PLACEMENT_3D('',#9211,#7210,#7211);
#6045=AXIS2_PLACEMENT_3D('',#9213,#7212,#7213);
#6046=AXIS2_PLACEMENT_3D('',#9215,#7214,#7215);
#6047=AXIS2_PLACEMENT_3D('',#9216,#7216,#7217);
#6048=AXIS2_PLACEMENT_3D('',#9217,#7218,#7219);
#6049=AXIS2_PLACEMENT_3D('',#9220,#7220,#7221);
#6050=AXIS2_PLACEMENT_3D('',#9221,#7222,#7223);
#6051=AXIS2_PLACEMENT_3D('',#9222,#7224,#7225);
#6052=AXIS2_PLACEMENT_3D('',#9223,#7226,#7227);
#6053=AXIS2_PLACEMENT_3D('',#9225,#7228,#7229);
#6054=AXIS2_PLACEMENT_3D('',#9227,#7230,#7231);
#6055=AXIS2_PLACEMENT_3D('',#9228,#7232,#7233);
#6056=AXIS2_PLACEMENT_3D('',#9229,#7234,#7235);
#6057=AXIS2_PLACEMENT_3D('',#9232,#7238,#7239);
#6058=AXIS2_PLACEMENT_3D('',#9235,#7240,#7241);
#6059=AXIS2_PLACEMENT_3D('',#9236,#7242,#7243);
#6060=AXIS2_PLACEMENT_3D('',#9237,#7244,#7245);
#6061=AXIS2_PLACEMENT_3D('',#9238,#7246,#7247);
#6062=AXIS2_PLACEMENT_3D('',#9240,#7249,#7250);
#6063=AXIS2_PLACEMENT_3D('',#9243,#7251,#7252);
#6064=AXIS2_PLACEMENT_3D('',#9244,#7253,#7254);
#6065=AXIS2_PLACEMENT_3D('',#9245,#7255,#7256);
#6066=AXIS2_PLACEMENT_3D('',#9246,#7257,#7258);
#6067=AXIS2_PLACEMENT_3D('',#9248,#7260,#7261);
#6068=AXIS2_PLACEMENT_3D('',#9250,#7262,#7263);
#6069=AXIS2_PLACEMENT_3D('',#9252,#7264,#7265);
#6070=AXIS2_PLACEMENT_3D('',#9253,#7266,#7267);
#6071=AXIS2_PLACEMENT_3D('',#9254,#7268,#7269);
#6072=AXIS2_PLACEMENT_3D('',#9257,#7270,#7271);
#6073=AXIS2_PLACEMENT_3D('',#9258,#7272,#7273);
#6074=AXIS2_PLACEMENT_3D('',#9259,#7274,#7275);
#6075=AXIS2_PLACEMENT_3D('',#9260,#7276,#7277);
#6076=AXIS2_PLACEMENT_3D('',#9262,#7278,#7279);
#6077=AXIS2_PLACEMENT_3D('',#9264,#7280,#7281);
#6078=AXIS2_PLACEMENT_3D('',#9265,#7282,#7283);
#6079=AXIS2_PLACEMENT_3D('',#9266,#7284,#7285);
#6080=AXIS2_PLACEMENT_3D('',#9269,#7288,#7289);
#6081=AXIS2_PLACEMENT_3D('',#9271,#7291,#7292);
#6082=AXIS2_PLACEMENT_3D('',#9273,#7293,#7294);
#6083=AXIS2_PLACEMENT_3D('',#9275,#7295,#7296);
#6084=AXIS2_PLACEMENT_3D('',#9276,#7297,#7298);
#6085=AXIS2_PLACEMENT_3D('',#9277,#7299,#7300);
#6086=AXIS2_PLACEMENT_3D('',#9279,#7301,#7302);
#6087=AXIS2_PLACEMENT_3D('',#9280,#7303,#7304);
#6088=AXIS2_PLACEMENT_3D('',#9281,#7305,#7306);
#6089=AXIS2_PLACEMENT_3D('',#9282,#7307,#7308);
#6090=AXIS2_PLACEMENT_3D('',#9284,#7309,#7310);
#6091=AXIS2_PLACEMENT_3D('',#9286,#7311,#7312);
#6092=AXIS2_PLACEMENT_3D('',#9287,#7313,#7314);
#6093=AXIS2_PLACEMENT_3D('',#9288,#7315,#7316);
#6094=AXIS2_PLACEMENT_3D('',#9291,#7319,#7320);
#6095=AXIS2_PLACEMENT_3D('',#9292,#7321,#7322);
#6096=AXIS2_PLACEMENT_3D('',#9294,#7323,#7324);
#6097=AXIS2_PLACEMENT_3D('',#9295,#7325,#7326);
#6098=AXIS2_PLACEMENT_3D('',#9296,#7327,#7328);
#6099=AXIS2_PLACEMENT_3D('',#9298,#7330,#7331);
#6100=AXIS2_PLACEMENT_3D('',#9300,#7333,#7334);
#6101=AXIS2_PLACEMENT_3D('',#9301,#7335,#7336);
#6102=AXIS2_PLACEMENT_3D('',#9303,#7337,#7338);
#6103=AXIS2_PLACEMENT_3D('',#9304,#7339,#7340);
#6104=AXIS2_PLACEMENT_3D('',#9305,#7341,#7342);
#6105=AXIS2_PLACEMENT_3D('',#9307,#7343,#7344);
#6106=AXIS2_PLACEMENT_3D('',#9308,#7345,#7346);
#6107=AXIS2_PLACEMENT_3D('',#9309,#7347,#7348);
#6108=AXIS2_PLACEMENT_3D('',#9310,#7349,#7350);
#6109=AXIS2_PLACEMENT_3D('',#9312,#7352,#7353);
#6110=AXIS2_PLACEMENT_3D('',#9313,#7354,#7355);
#6111=AXIS2_PLACEMENT_3D('',#9315,#7357,#7358);
#6112=AXIS2_PLACEMENT_3D('',#9317,#7360,#7361);
#6113=AXIS2_PLACEMENT_3D('',#9318,#7362,#7363);
#6114=AXIS2_PLACEMENT_3D('',#9320,#7365,#7366);
#6115=AXIS2_PLACEMENT_3D('',#9322,#7368,#7369);
#6116=AXIS2_PLACEMENT_3D('',#9324,#7371,#7372);
#6117=AXIS2_PLACEMENT_3D('',#9326,#7374,#7375);
#6118=AXIS2_PLACEMENT_3D('',#9329,#7378,#7379);
#6119=AXIS2_PLACEMENT_3D('',#9331,#7381,#7382);
#6120=AXIS2_PLACEMENT_3D('',#9334,#7385,#7386);
#6121=AXIS2_PLACEMENT_3D('',#9336,#7388,#7389);
#6122=AXIS2_PLACEMENT_3D('',#9338,#7391,#7392);
#6123=AXIS2_PLACEMENT_3D('',#9340,#7394,#7395);
#6124=AXIS2_PLACEMENT_3D('',#9342,#7397,#7398);
#6125=AXIS2_PLACEMENT_3D('',#9345,#7401,#7402);
#6126=AXIS2_PLACEMENT_3D('',#9347,#7404,#7405);
#6127=AXIS2_PLACEMENT_3D('',#9349,#7407,#7408);
#6128=AXIS2_PLACEMENT_3D('',#9352,#7411,#7412);
#6129=AXIS2_PLACEMENT_3D('',#9354,#7414,#7415);
#6130=AXIS2_PLACEMENT_3D('',#9356,#7417,#7418);
#6131=AXIS2_PLACEMENT_3D('',#9359,#7420,#7421);
#6132=AXIS2_PLACEMENT_3D('',#9360,#7422,#7423);
#6133=AXIS2_PLACEMENT_3D('',#9362,#7425,#7426);
#6134=AXIS2_PLACEMENT_3D('',#9365,#7428,#7429);
#6135=AXIS2_PLACEMENT_3D('',#9366,#7430,#7431);
#6136=AXIS2_PLACEMENT_3D('',#9368,#7433,#7434);
#6137=AXIS2_PLACEMENT_3D('',#9371,#7436,#7437);
#6138=AXIS2_PLACEMENT_3D('',#9372,#7438,#7439);
#6139=AXIS2_PLACEMENT_3D('',#9374,#7441,#7442);
#6140=AXIS2_PLACEMENT_3D('',#9377,#7445,#7446);
#6141=AXIS2_PLACEMENT_3D('',#9379,#7448,#7449);
#6142=AXIS2_PLACEMENT_3D('',#9381,#7451,#7452);
#6143=AXIS2_PLACEMENT_3D('',#9383,#7454,#7455);
#6144=AXIS2_PLACEMENT_3D('',#9385,#7457,#7458);
#6145=AXIS2_PLACEMENT_3D('',#9387,#7460,#7461);
#6146=AXIS2_PLACEMENT_3D('',#9389,#7463,#7464);
#6147=AXIS2_PLACEMENT_3D('',#9390,#7465,#7466);
#6148=AXIS2_PLACEMENT_3D('',#9391,#7467,#7468);
#6149=AXIS2_PLACEMENT_3D('',#9392,#7469,#7470);
#6150=AXIS2_PLACEMENT_3D('',#9393,#7471,#7472);
#6151=AXIS2_PLACEMENT_3D('',#9394,#7473,#7474);
#6152=AXIS2_PLACEMENT_3D('',#9395,#7475,#7476);
#6153=AXIS2_PLACEMENT_3D('',#9396,#7477,#7478);
#6154=AXIS2_PLACEMENT_3D('',#9397,#7479,#7480);
#6155=AXIS2_PLACEMENT_3D('',#9398,#7481,#7482);
#6156=AXIS2_PLACEMENT_3D('',#9399,#7483,#7484);
#6157=AXIS2_PLACEMENT_3D('',#9400,#7485,#7486);
#6158=AXIS2_PLACEMENT_3D('',#9401,#7487,#7488);
#6159=AXIS2_PLACEMENT_3D('',#9402,#7489,#7490);
#6160=AXIS2_PLACEMENT_3D('',#9403,#7491,#7492);
#6161=AXIS2_PLACEMENT_3D('',#9404,#7493,#7494);
#6162=AXIS2_PLACEMENT_3D('',#9405,#7495,#7496);
#6163=AXIS2_PLACEMENT_3D('',#9406,#7497,#7498);
#6164=AXIS2_PLACEMENT_3D('',#9407,#7499,#7500);
#6165=AXIS2_PLACEMENT_3D('',#9408,#7501,#7502);
#6166=AXIS2_PLACEMENT_3D('',#9409,#7503,#7504);
#6167=AXIS2_PLACEMENT_3D('',#9410,#7505,#7506);
#6168=AXIS2_PLACEMENT_3D('',#9411,#7507,#7508);
#6169=AXIS2_PLACEMENT_3D('',#9412,#7509,#7510);
#6170=AXIS2_PLACEMENT_3D('',#9413,#7511,#7512);
#6171=AXIS2_PLACEMENT_3D('',#9414,#7513,#7514);
#6172=AXIS2_PLACEMENT_3D('',#9415,#7515,#7516);
#6173=AXIS2_PLACEMENT_3D('',#9416,#7517,#7518);
#6174=AXIS2_PLACEMENT_3D('',#9417,#7519,#7520);
#6175=AXIS2_PLACEMENT_3D('',#9418,#7521,#7522);
#6176=AXIS2_PLACEMENT_3D('',#9420,#7523,#7524);
#6177=AXIS2_PLACEMENT_3D('',#9422,#7525,#7526);
#6178=AXIS2_PLACEMENT_3D('',#9424,#7527,#7528);
#6179=AXIS2_PLACEMENT_3D('',#9425,#7529,#7530);
#6180=AXIS2_PLACEMENT_3D('',#9426,#7531,#7532);
#6181=AXIS2_PLACEMENT_3D('',#9428,#7533,#7534);
#6182=AXIS2_PLACEMENT_3D('',#9429,#7535,#7536);
#6183=AXIS2_PLACEMENT_3D('',#9433,#7538,#7539);
#6184=AXIS2_PLACEMENT_3D('',#9434,#7540,#7541);
#6185=AXIS2_PLACEMENT_3D('',#9435,#7542,#7543);
#6186=AXIS2_PLACEMENT_3D('',#9437,#7544,#7545);
#6187=AXIS2_PLACEMENT_3D('',#9439,#7546,#7547);
#6188=AXIS2_PLACEMENT_3D('',#9440,#7548,#7549);
#6189=AXIS2_PLACEMENT_3D('',#9441,#7550,#7551);
#6190=AXIS2_PLACEMENT_3D('',#9445,#7553,#7554);
#6191=AXIS2_PLACEMENT_3D('',#9446,#7555,#7556);
#6192=AXIS2_PLACEMENT_3D('',#9447,#7557,#7558);
#6193=AXIS2_PLACEMENT_3D('',#9449,#7559,#7560);
#6194=AXIS2_PLACEMENT_3D('',#9450,#7561,#7562);
#6195=AXIS2_PLACEMENT_3D('',#9451,#7563,#7564);
#6196=AXIS2_PLACEMENT_3D('',#9453,#7565,#7566);
#6197=AXIS2_PLACEMENT_3D('',#9454,#7567,#7568);
#6198=AXIS2_PLACEMENT_3D('',#9455,#7569,#7570);
#6199=AXIS2_PLACEMENT_3D('',#9456,#7571,#7572);
#6200=AXIS2_PLACEMENT_3D('',#9457,#7573,#7574);
#6201=AXIS2_PLACEMENT_3D('',#9459,#7575,#7576);
#6202=AXIS2_PLACEMENT_3D('',#9461,#7577,#7578);
#6203=AXIS2_PLACEMENT_3D('',#9463,#7579,#7580);
#6204=AXIS2_PLACEMENT_3D('',#9464,#7581,#7582);
#6205=AXIS2_PLACEMENT_3D('',#9465,#7583,#7584);
#6206=AXIS2_PLACEMENT_3D('',#9467,#7585,#7586);
#6207=AXIS2_PLACEMENT_3D('',#9468,#7587,#7588);
#6208=AXIS2_PLACEMENT_3D('',#9472,#7590,#7591);
#6209=AXIS2_PLACEMENT_3D('',#9473,#7592,#7593);
#6210=AXIS2_PLACEMENT_3D('',#9474,#7594,#7595);
#6211=AXIS2_PLACEMENT_3D('',#9476,#7596,#7597);
#6212=AXIS2_PLACEMENT_3D('',#9478,#7598,#7599);
#6213=AXIS2_PLACEMENT_3D('',#9479,#7600,#7601);
#6214=AXIS2_PLACEMENT_3D('',#9480,#7602,#7603);
#6215=AXIS2_PLACEMENT_3D('',#9484,#7605,#7606);
#6216=AXIS2_PLACEMENT_3D('',#9485,#7607,#7608);
#6217=AXIS2_PLACEMENT_3D('',#9486,#7609,#7610);
#6218=AXIS2_PLACEMENT_3D('',#9488,#7611,#7612);
#6219=AXIS2_PLACEMENT_3D('',#9489,#7613,#7614);
#6220=AXIS2_PLACEMENT_3D('',#9490,#7615,#7616);
#6221=AXIS2_PLACEMENT_3D('',#9492,#7617,#7618);
#6222=AXIS2_PLACEMENT_3D('',#9493,#7619,#7620);
#6223=AXIS2_PLACEMENT_3D('',#9494,#7621,#7622);
#6224=AXIS2_PLACEMENT_3D('',#9495,#7623,#7624);
#6225=AXIS2_PLACEMENT_3D('',#9496,#7625,#7626);
#6226=AXIS2_PLACEMENT_3D('',#9498,#7627,#7628);
#6227=AXIS2_PLACEMENT_3D('',#9500,#7629,#7630);
#6228=AXIS2_PLACEMENT_3D('',#9501,#7631,#7632);
#6229=AXIS2_PLACEMENT_3D('',#9502,#7633,#7634);
#6230=AXIS2_PLACEMENT_3D('',#9512,#7639,#7640);
#6231=AXIS2_PLACEMENT_3D('',#9513,#7641,#7642);
#6232=AXIS2_PLACEMENT_3D('',#9516,#7644,#7645);
#6233=AXIS2_PLACEMENT_3D('',#9517,#7646,#7647);
#6234=AXIS2_PLACEMENT_3D('',#9519,#7648,#7649);
#6235=AXIS2_PLACEMENT_3D('',#9520,#7650,#7651);
#6236=AXIS2_PLACEMENT_3D('',#9521,#7652,#7653);
#6237=AXIS2_PLACEMENT_3D('',#9524,#7655,#7656);
#6238=AXIS2_PLACEMENT_3D('',#9525,#7657,#7658);
#6239=AXIS2_PLACEMENT_3D('',#9527,#7659,#7660);
#6240=AXIS2_PLACEMENT_3D('',#9529,#7661,#7662);
#6241=AXIS2_PLACEMENT_3D('',#9531,#7663,#7664);
#6242=AXIS2_PLACEMENT_3D('',#9532,#7665,#7666);
#6243=AXIS2_PLACEMENT_3D('',#9533,#7667,#7668);
#6244=AXIS2_PLACEMENT_3D('',#9543,#7673,#7674);
#6245=AXIS2_PLACEMENT_3D('',#9544,#7675,#7676);
#6246=AXIS2_PLACEMENT_3D('',#9547,#7678,#7679);
#6247=AXIS2_PLACEMENT_3D('',#9548,#7680,#7681);
#6248=AXIS2_PLACEMENT_3D('',#9550,#7682,#7683);
#6249=AXIS2_PLACEMENT_3D('',#9552,#7684,#7685);
#6250=AXIS2_PLACEMENT_3D('',#9553,#7686,#7687);
#6251=AXIS2_PLACEMENT_3D('',#9554,#7688,#7689);
#6252=AXIS2_PLACEMENT_3D('',#9557,#7691,#7692);
#6253=AXIS2_PLACEMENT_3D('',#9558,#7693,#7694);
#6254=AXIS2_PLACEMENT_3D('',#9561,#7695,#7696);
#6255=AXIS2_PLACEMENT_3D('',#9563,#7697,#7698);
#6256=AXIS2_PLACEMENT_3D('',#9564,#7699,#7700);
#6257=AXIS2_PLACEMENT_3D('',#9565,#7701,#7702);
#6258=AXIS2_PLACEMENT_3D('',#9568,#7703,#7704);
#6259=AXIS2_PLACEMENT_3D('',#9570,#7705,#7706);
#6260=AXIS2_PLACEMENT_3D('',#9571,#7707,#7708);
#6261=AXIS2_PLACEMENT_3D('',#9572,#7709,#7710);
#6262=AXIS2_PLACEMENT_3D('',#9575,#7711,#7712);
#6263=AXIS2_PLACEMENT_3D('',#9577,#7713,#7714);
#6264=AXIS2_PLACEMENT_3D('',#9578,#7715,#7716);
#6265=AXIS2_PLACEMENT_3D('',#9579,#7717,#7718);
#6266=AXIS2_PLACEMENT_3D('',#9582,#7721,#7722);
#6267=AXIS2_PLACEMENT_3D('',#9584,#7723,#7724);
#6268=AXIS2_PLACEMENT_3D('',#9586,#7725,#7726);
#6269=AXIS2_PLACEMENT_3D('',#9587,#7727,#7728);
#6270=AXIS2_PLACEMENT_3D('',#9588,#7729,#7730);
#6271=AXIS2_PLACEMENT_3D('',#9591,#7733,#7734);
#6272=AXIS2_PLACEMENT_3D('',#9594,#7735,#7736);
#6273=AXIS2_PLACEMENT_3D('',#9596,#7737,#7738);
#6274=AXIS2_PLACEMENT_3D('',#9597,#7739,#7740);
#6275=AXIS2_PLACEMENT_3D('',#9598,#7741,#7742);
#6276=AXIS2_PLACEMENT_3D('',#9601,#7745,#7746);
#6277=AXIS2_PLACEMENT_3D('',#9604,#7749,#7750);
#6278=AXIS2_PLACEMENT_3D('',#9606,#7751,#7752);
#6279=AXIS2_PLACEMENT_3D('',#9608,#7753,#7754);
#6280=AXIS2_PLACEMENT_3D('',#9609,#7755,#7756);
#6281=AXIS2_PLACEMENT_3D('',#9610,#7757,#7758);
#6282=AXIS2_PLACEMENT_3D('',#9613,#7761,#7762);
#6283=AXIS2_PLACEMENT_3D('',#9616,#7763,#7764);
#6284=AXIS2_PLACEMENT_3D('',#9617,#7765,#7766);
#6285=AXIS2_PLACEMENT_3D('',#9618,#7767,#7768);
#6286=AXIS2_PLACEMENT_3D('',#9619,#7769,#7770);
#6287=AXIS2_PLACEMENT_3D('',#9621,#7771,#7772);
#6288=AXIS2_PLACEMENT_3D('',#9623,#7773,#7774);
#6289=AXIS2_PLACEMENT_3D('',#9625,#7775,#7776);
#6290=AXIS2_PLACEMENT_3D('',#9626,#7777,#7778);
#6291=AXIS2_PLACEMENT_3D('',#9627,#7779,#7780);
#6292=AXIS2_PLACEMENT_3D('',#9630,#7781,#7782);
#6293=AXIS2_PLACEMENT_3D('',#9631,#7783,#7784);
#6294=AXIS2_PLACEMENT_3D('',#9632,#7785,#7786);
#6295=AXIS2_PLACEMENT_3D('',#9633,#7787,#7788);
#6296=AXIS2_PLACEMENT_3D('',#9635,#7790,#7791);
#6297=AXIS2_PLACEMENT_3D('',#9638,#7792,#7793);
#6298=AXIS2_PLACEMENT_3D('',#9639,#7794,#7795);
#6299=AXIS2_PLACEMENT_3D('',#9641,#7796,#7797);
#6300=AXIS2_PLACEMENT_3D('',#9642,#7798,#7799);
#6301=AXIS2_PLACEMENT_3D('',#9643,#7800,#7801);
#6302=AXIS2_PLACEMENT_3D('',#9646,#7802,#7803);
#6303=AXIS2_PLACEMENT_3D('',#9647,#7804,#7805);
#6304=AXIS2_PLACEMENT_3D('',#9649,#7806,#7807);
#6305=AXIS2_PLACEMENT_3D('',#9650,#7808,#7809);
#6306=AXIS2_PLACEMENT_3D('',#9651,#7810,#7811);
#6307=AXIS2_PLACEMENT_3D('',#9654,#7812,#7813);
#6308=AXIS2_PLACEMENT_3D('',#9656,#7814,#7815);
#6309=AXIS2_PLACEMENT_3D('',#9657,#7816,#7817);
#6310=AXIS2_PLACEMENT_3D('',#9658,#7818,#7819);
#6311=AXIS2_PLACEMENT_3D('',#9661,#7822,#7823);
#6312=AXIS2_PLACEMENT_3D('',#9663,#7824,#7825);
#6313=AXIS2_PLACEMENT_3D('',#9665,#7826,#7827);
#6314=AXIS2_PLACEMENT_3D('',#9667,#7828,#7829);
#6315=AXIS2_PLACEMENT_3D('',#9668,#7830,#7831);
#6316=AXIS2_PLACEMENT_3D('',#9669,#7832,#7833);
#6317=AXIS2_PLACEMENT_3D('',#9672,#7834,#7835);
#6318=AXIS2_PLACEMENT_3D('',#9674,#7836,#7837);
#6319=AXIS2_PLACEMENT_3D('',#9675,#7838,#7839);
#6320=AXIS2_PLACEMENT_3D('',#9676,#7840,#7841);
#6321=AXIS2_PLACEMENT_3D('',#9679,#7844,#7845);
#6322=AXIS2_PLACEMENT_3D('',#9682,#7846,#7847);
#6323=AXIS2_PLACEMENT_3D('',#9684,#7848,#7849);
#6324=AXIS2_PLACEMENT_3D('',#9685,#7850,#7851);
#6325=AXIS2_PLACEMENT_3D('',#9686,#7852,#7853);
#6326=AXIS2_PLACEMENT_3D('',#9689,#7856,#7857);
#6327=AXIS2_PLACEMENT_3D('',#9692,#7858,#7859);
#6328=AXIS2_PLACEMENT_3D('',#9694,#7860,#7861);
#6329=AXIS2_PLACEMENT_3D('',#9695,#7862,#7863);
#6330=AXIS2_PLACEMENT_3D('',#9696,#7864,#7865);
#6331=AXIS2_PLACEMENT_3D('',#9699,#7868,#7869);
#6332=AXIS2_PLACEMENT_3D('',#9702,#7870,#7871);
#6333=AXIS2_PLACEMENT_3D('',#9704,#7872,#7873);
#6334=AXIS2_PLACEMENT_3D('',#9705,#7874,#7875);
#6335=AXIS2_PLACEMENT_3D('',#9706,#7876,#7877);
#6336=AXIS2_PLACEMENT_3D('',#9709,#7880,#7881);
#6337=AXIS2_PLACEMENT_3D('',#9712,#7884,#7885);
#6338=AXIS2_PLACEMENT_3D('',#9715,#7886,#7887);
#6339=AXIS2_PLACEMENT_3D('',#9717,#7888,#7889);
#6340=AXIS2_PLACEMENT_3D('',#9718,#7890,#7891);
#6341=AXIS2_PLACEMENT_3D('',#9719,#7892,#7893);
#6342=AXIS2_PLACEMENT_3D('',#9722,#7894,#7895);
#6343=AXIS2_PLACEMENT_3D('',#9724,#7896,#7897);
#6344=AXIS2_PLACEMENT_3D('',#9725,#7898,#7899);
#6345=AXIS2_PLACEMENT_3D('',#9726,#7900,#7901);
#6346=AXIS2_PLACEMENT_3D('',#9745,#7904,#7905);
#6347=AXIS2_PLACEMENT_3D('',#9748,#7906,#7907);
#6348=AXIS2_PLACEMENT_3D('',#9750,#7908,#7909);
#6349=AXIS2_PLACEMENT_3D('',#9751,#7910,#7911);
#6350=AXIS2_PLACEMENT_3D('',#9752,#7912,#7913);
#6351=AXIS2_PLACEMENT_3D('',#9755,#7916,#7917);
#6352=AXIS2_PLACEMENT_3D('',#9758,#7920,#7921);
#6353=AXIS2_PLACEMENT_3D('',#9777,#7924,#7925);
#6354=AXIS2_PLACEMENT_3D('',#9796,#7928,#7929);
#6355=AXIS2_PLACEMENT_3D('',#9815,#7932,#7933);
#6356=AXIS2_PLACEMENT_3D('',#9818,#7934,#7935);
#6357=AXIS2_PLACEMENT_3D('',#9820,#7936,#7937);
#6358=AXIS2_PLACEMENT_3D('',#9821,#7938,#7939);
#6359=AXIS2_PLACEMENT_3D('',#9822,#7940,#7941);
#6360=AXIS2_PLACEMENT_3D('',#9825,#7942,#7943);
#6361=AXIS2_PLACEMENT_3D('',#9827,#7944,#7945);
#6362=AXIS2_PLACEMENT_3D('',#9828,#7946,#7947);
#6363=AXIS2_PLACEMENT_3D('',#9829,#7948,#7949);
#6364=AXIS2_PLACEMENT_3D('',#9832,#7950,#7951);
#6365=AXIS2_PLACEMENT_3D('',#9834,#7952,#7953);
#6366=AXIS2_PLACEMENT_3D('',#9835,#7954,#7955);
#6367=AXIS2_PLACEMENT_3D('',#9836,#7956,#7957);
#6368=AXIS2_PLACEMENT_3D('',#9839,#7960,#7961);
#6369=AXIS2_PLACEMENT_3D('',#9842,#7962,#7963);
#6370=AXIS2_PLACEMENT_3D('',#9844,#7964,#7965);
#6371=AXIS2_PLACEMENT_3D('',#9845,#7966,#7967);
#6372=AXIS2_PLACEMENT_3D('',#9846,#7968,#7969);
#6373=AXIS2_PLACEMENT_3D('',#9865,#7972,#7973);
#6374=AXIS2_PLACEMENT_3D('',#9868,#7976,#7977);
#6375=AXIS2_PLACEMENT_3D('',#9871,#7980,#7981);
#6376=AXIS2_PLACEMENT_3D('',#9890,#7984,#7985);
#6377=AXIS2_PLACEMENT_3D('',#9893,#7988,#7989);
#6378=AXIS2_PLACEMENT_3D('',#9912,#7992,#7993);
#6379=AXIS2_PLACEMENT_3D('',#9913,#7994,#7995);
#6380=AXIS2_PLACEMENT_3D('',#9914,#7996,#7997);
#6381=AXIS2_PLACEMENT_3D('',#9915,#7998,#7999);
#6382=AXIS2_PLACEMENT_3D('',#9934,#8002,#8003);
#6383=AXIS2_PLACEMENT_3D('',#9935,#8004,#8005);
#6384=AXIS2_PLACEMENT_3D('',#9936,#8006,#8007);
#6385=AXIS2_PLACEMENT_3D('',#9937,#8008,#8009);
#6386=AXIS2_PLACEMENT_3D('',#9938,#8010,#8011);
#6387=AXIS2_PLACEMENT_3D('',#9939,#8012,#8013);
#6388=AXIS2_PLACEMENT_3D('',#9940,#8014,#8015);
#6389=AXIS2_PLACEMENT_3D('',#9941,#8016,#8017);
#6390=AXIS2_PLACEMENT_3D('',#9942,#8018,#8019);
#6391=AXIS2_PLACEMENT_3D('',#9943,#8020,#8021);
#6392=AXIS2_PLACEMENT_3D('',#9946,#8024,#8025);
#6393=AXIS2_PLACEMENT_3D('',#9949,#8028,#8029);
#6394=AXIS2_PLACEMENT_3D('',#9952,#8032,#8033);
#6395=AXIS2_PLACEMENT_3D('',#9955,#8036,#8037);
#6396=AXIS2_PLACEMENT_3D('',#9957,#8039,#8040);
#6397=AXIS2_PLACEMENT_3D('',#9959,#8042,#8043);
#6398=AXIS2_PLACEMENT_3D('',#9961,#8045,#8046);
#6399=AXIS2_PLACEMENT_3D('',#9963,#8048,#8049);
#6400=AXIS2_PLACEMENT_3D('',#9965,#8051,#8052);
#6401=AXIS2_PLACEMENT_3D('',#9968,#8055,#8056);
#6402=AXIS2_PLACEMENT_3D('',#9970,#8058,#8059);
#6403=AXIS2_PLACEMENT_3D('',#9973,#8062,#8063);
#6404=AXIS2_PLACEMENT_3D('',#9975,#8065,#8066);
#6405=AXIS2_PLACEMENT_3D('',#9978,#8069,#8070);
#6406=AXIS2_PLACEMENT_3D('',#9980,#8072,#8073);
#6407=AXIS2_PLACEMENT_3D('',#9982,#8075,#8076);
#6408=AXIS2_PLACEMENT_3D('',#9985,#8079,#8080);
#6409=AXIS2_PLACEMENT_3D('',#9986,#8081,#8082);
#6410=AXIS2_PLACEMENT_3D('',#9987,#8083,#8084);
#6411=AXIS2_PLACEMENT_3D('',#9988,#8085,#8086);
#6412=AXIS2_PLACEMENT_3D('',#9989,#8087,#8088);
#6413=AXIS2_PLACEMENT_3D('',#9990,#8089,#8090);
#6414=AXIS2_PLACEMENT_3D('',#9991,#8091,#8092);
#6415=AXIS2_PLACEMENT_3D('',#9992,#8093,#8094);
#6416=AXIS2_PLACEMENT_3D('',#9993,#8095,#8096);
#6417=AXIS2_PLACEMENT_3D('',#9994,#8097,#8098);
#6418=AXIS2_PLACEMENT_3D('',#9995,#8099,#8100);
#6419=AXIS2_PLACEMENT_3D('',#9996,#8101,#8102);
#6420=AXIS2_PLACEMENT_3D('',#9997,#8103,#8104);
#6421=AXIS2_PLACEMENT_3D('',#9998,#8105,#8106);
#6422=AXIS2_PLACEMENT_3D('',#9999,#8107,#8108);
#6423=AXIS2_PLACEMENT_3D('',#10001,#8109,#8110);
#6424=AXIS2_PLACEMENT_3D('',#10002,#8111,#8112);
#6425=AXIS2_PLACEMENT_3D('',#10004,#8113,#8114);
#6426=AXIS2_PLACEMENT_3D('',#10006,#8116,#8117);
#6427=AXIS2_PLACEMENT_3D('',#10007,#8118,#8119);
#6428=AXIS2_PLACEMENT_3D('',#10008,#8120,#8121);
#6429=AXIS2_PLACEMENT_3D('',#10010,#8122,#8123);
#6430=AXIS2_PLACEMENT_3D('',#10012,#8124,#8125);
#6431=AXIS2_PLACEMENT_3D('',#10014,#8126,#8127);
#6432=AXIS2_PLACEMENT_3D('',#10015,#8128,#8129);
#6433=AXIS2_PLACEMENT_3D('',#10016,#8130,#8131);
#6434=AXIS2_PLACEMENT_3D('',#10018,#8132,#8133);
#6435=AXIS2_PLACEMENT_3D('',#10019,#8134,#8135);
#6436=AXIS2_PLACEMENT_3D('',#10023,#8137,#8138);
#6437=AXIS2_PLACEMENT_3D('',#10024,#8139,#8140);
#6438=AXIS2_PLACEMENT_3D('',#10025,#8141,#8142);
#6439=AXIS2_PLACEMENT_3D('',#10027,#8143,#8144);
#6440=AXIS2_PLACEMENT_3D('',#10029,#8145,#8146);
#6441=AXIS2_PLACEMENT_3D('',#10030,#8147,#8148);
#6442=AXIS2_PLACEMENT_3D('',#10031,#8149,#8150);
#6443=AXIS2_PLACEMENT_3D('',#10035,#8152,#8153);
#6444=AXIS2_PLACEMENT_3D('',#10036,#8154,#8155);
#6445=AXIS2_PLACEMENT_3D('',#10037,#8156,#8157);
#6446=AXIS2_PLACEMENT_3D('',#10039,#8158,#8159);
#6447=AXIS2_PLACEMENT_3D('',#10040,#8160,#8161);
#6448=AXIS2_PLACEMENT_3D('',#10041,#8162,#8163);
#6449=AXIS2_PLACEMENT_3D('',#10043,#8164,#8165);
#6450=AXIS2_PLACEMENT_3D('',#10044,#8166,#8167);
#6451=AXIS2_PLACEMENT_3D('',#10045,#8168,#8169);
#6452=AXIS2_PLACEMENT_3D('',#10046,#8170,#8171);
#6453=AXIS2_PLACEMENT_3D('',#10047,#8172,#8173);
#6454=AXIS2_PLACEMENT_3D('',#10049,#8174,#8175);
#6455=AXIS2_PLACEMENT_3D('',#10050,#8176,#8177);
#6456=AXIS2_PLACEMENT_3D('',#10052,#8178,#8179);
#6457=AXIS2_PLACEMENT_3D('',#10054,#8181,#8182);
#6458=AXIS2_PLACEMENT_3D('',#10055,#8183,#8184);
#6459=AXIS2_PLACEMENT_3D('',#10056,#8185,#8186);
#6460=AXIS2_PLACEMENT_3D('',#10058,#8187,#8188);
#6461=AXIS2_PLACEMENT_3D('',#10059,#8189,#8190);
#6462=AXIS2_PLACEMENT_3D('',#10061,#8191,#8192);
#6463=AXIS2_PLACEMENT_3D('',#10063,#8194,#8195);
#6464=AXIS2_PLACEMENT_3D('',#10064,#8196,#8197);
#6465=AXIS2_PLACEMENT_3D('',#10065,#8198,#8199);
#6466=AXIS2_PLACEMENT_3D('',#10067,#8200,#8201);
#6467=AXIS2_PLACEMENT_3D('',#10069,#8202,#8203);
#6468=AXIS2_PLACEMENT_3D('',#10071,#8204,#8205);
#6469=AXIS2_PLACEMENT_3D('',#10072,#8206,#8207);
#6470=AXIS2_PLACEMENT_3D('',#10073,#8208,#8209);
#6471=AXIS2_PLACEMENT_3D('',#10075,#8210,#8211);
#6472=AXIS2_PLACEMENT_3D('',#10076,#8212,#8213);
#6473=AXIS2_PLACEMENT_3D('',#10080,#8215,#8216);
#6474=AXIS2_PLACEMENT_3D('',#10081,#8217,#8218);
#6475=AXIS2_PLACEMENT_3D('',#10082,#8219,#8220);
#6476=AXIS2_PLACEMENT_3D('',#10084,#8221,#8222);
#6477=AXIS2_PLACEMENT_3D('',#10086,#8223,#8224);
#6478=AXIS2_PLACEMENT_3D('',#10087,#8225,#8226);
#6479=AXIS2_PLACEMENT_3D('',#10088,#8227,#8228);
#6480=AXIS2_PLACEMENT_3D('',#10092,#8230,#8231);
#6481=AXIS2_PLACEMENT_3D('',#10093,#8232,#8233);
#6482=AXIS2_PLACEMENT_3D('',#10094,#8234,#8235);
#6483=AXIS2_PLACEMENT_3D('',#10096,#8236,#8237);
#6484=AXIS2_PLACEMENT_3D('',#10097,#8238,#8239);
#6485=AXIS2_PLACEMENT_3D('',#10098,#8240,#8241);
#6486=AXIS2_PLACEMENT_3D('',#10100,#8242,#8243);
#6487=AXIS2_PLACEMENT_3D('',#10101,#8244,#8245);
#6488=AXIS2_PLACEMENT_3D('',#10102,#8246,#8247);
#6489=AXIS2_PLACEMENT_3D('',#10103,#8248,#8249);
#6490=AXIS2_PLACEMENT_3D('',#10104,#8250,#8251);
#6491=AXIS2_PLACEMENT_3D('',#10106,#8252,#8253);
#6492=AXIS2_PLACEMENT_3D('',#10108,#8254,#8255);
#6493=AXIS2_PLACEMENT_3D('',#10109,#8256,#8257);
#6494=AXIS2_PLACEMENT_3D('',#10110,#8258,#8259);
#6495=AXIS2_PLACEMENT_3D('',#10120,#8264,#8265);
#6496=AXIS2_PLACEMENT_3D('',#10121,#8266,#8267);
#6497=AXIS2_PLACEMENT_3D('',#10124,#8269,#8270);
#6498=AXIS2_PLACEMENT_3D('',#10125,#8271,#8272);
#6499=AXIS2_PLACEMENT_3D('',#10127,#8273,#8274);
#6500=AXIS2_PLACEMENT_3D('',#10128,#8275,#8276);
#6501=AXIS2_PLACEMENT_3D('',#10129,#8277,#8278);
#6502=AXIS2_PLACEMENT_3D('',#10132,#8280,#8281);
#6503=AXIS2_PLACEMENT_3D('',#10133,#8282,#8283);
#6504=AXIS2_PLACEMENT_3D('',#10135,#8284,#8285);
#6505=AXIS2_PLACEMENT_3D('',#10137,#8286,#8287);
#6506=AXIS2_PLACEMENT_3D('',#10139,#8288,#8289);
#6507=AXIS2_PLACEMENT_3D('',#10140,#8290,#8291);
#6508=AXIS2_PLACEMENT_3D('',#10141,#8292,#8293);
#6509=AXIS2_PLACEMENT_3D('',#10151,#8298,#8299);
#6510=AXIS2_PLACEMENT_3D('',#10152,#8300,#8301);
#6511=AXIS2_PLACEMENT_3D('',#10155,#8303,#8304);
#6512=AXIS2_PLACEMENT_3D('',#10156,#8305,#8306);
#6513=AXIS2_PLACEMENT_3D('',#10158,#8307,#8308);
#6514=AXIS2_PLACEMENT_3D('',#10160,#8309,#8310);
#6515=AXIS2_PLACEMENT_3D('',#10161,#8311,#8312);
#6516=AXIS2_PLACEMENT_3D('',#10162,#8313,#8314);
#6517=AXIS2_PLACEMENT_3D('',#10165,#8316,#8317);
#6518=AXIS2_PLACEMENT_3D('',#10166,#8318,#8319);
#6519=AXIS2_PLACEMENT_3D('',#10169,#8320,#8321);
#6520=AXIS2_PLACEMENT_3D('',#10171,#8322,#8323);
#6521=AXIS2_PLACEMENT_3D('',#10172,#8324,#8325);
#6522=AXIS2_PLACEMENT_3D('',#10173,#8326,#8327);
#6523=AXIS2_PLACEMENT_3D('',#10176,#8328,#8329);
#6524=AXIS2_PLACEMENT_3D('',#10178,#8330,#8331);
#6525=AXIS2_PLACEMENT_3D('',#10179,#8332,#8333);
#6526=AXIS2_PLACEMENT_3D('',#10180,#8334,#8335);
#6527=AXIS2_PLACEMENT_3D('',#10183,#8336,#8337);
#6528=AXIS2_PLACEMENT_3D('',#10185,#8338,#8339);
#6529=AXIS2_PLACEMENT_3D('',#10186,#8340,#8341);
#6530=AXIS2_PLACEMENT_3D('',#10187,#8342,#8343);
#6531=AXIS2_PLACEMENT_3D('',#10190,#8346,#8347);
#6532=AXIS2_PLACEMENT_3D('',#10192,#8348,#8349);
#6533=AXIS2_PLACEMENT_3D('',#10194,#8350,#8351);
#6534=AXIS2_PLACEMENT_3D('',#10195,#8352,#8353);
#6535=AXIS2_PLACEMENT_3D('',#10196,#8354,#8355);
#6536=AXIS2_PLACEMENT_3D('',#10199,#8358,#8359);
#6537=AXIS2_PLACEMENT_3D('',#10202,#8360,#8361);
#6538=AXIS2_PLACEMENT_3D('',#10204,#8362,#8363);
#6539=AXIS2_PLACEMENT_3D('',#10205,#8364,#8365);
#6540=AXIS2_PLACEMENT_3D('',#10206,#8366,#8367);
#6541=AXIS2_PLACEMENT_3D('',#10209,#8370,#8371);
#6542=AXIS2_PLACEMENT_3D('',#10212,#8374,#8375);
#6543=AXIS2_PLACEMENT_3D('',#10214,#8376,#8377);
#6544=AXIS2_PLACEMENT_3D('',#10216,#8378,#8379);
#6545=AXIS2_PLACEMENT_3D('',#10217,#8380,#8381);
#6546=AXIS2_PLACEMENT_3D('',#10218,#8382,#8383);
#6547=AXIS2_PLACEMENT_3D('',#10221,#8386,#8387);
#6548=AXIS2_PLACEMENT_3D('',#10224,#8388,#8389);
#6549=AXIS2_PLACEMENT_3D('',#10225,#8390,#8391);
#6550=AXIS2_PLACEMENT_3D('',#10226,#8392,#8393);
#6551=AXIS2_PLACEMENT_3D('',#10227,#8394,#8395);
#6552=AXIS2_PLACEMENT_3D('',#10229,#8396,#8397);
#6553=AXIS2_PLACEMENT_3D('',#10231,#8398,#8399);
#6554=AXIS2_PLACEMENT_3D('',#10233,#8400,#8401);
#6555=AXIS2_PLACEMENT_3D('',#10234,#8402,#8403);
#6556=AXIS2_PLACEMENT_3D('',#10235,#8404,#8405);
#6557=AXIS2_PLACEMENT_3D('',#10238,#8406,#8407);
#6558=AXIS2_PLACEMENT_3D('',#10239,#8408,#8409);
#6559=AXIS2_PLACEMENT_3D('',#10240,#8410,#8411);
#6560=AXIS2_PLACEMENT_3D('',#10241,#8412,#8413);
#6561=AXIS2_PLACEMENT_3D('',#10243,#8415,#8416);
#6562=AXIS2_PLACEMENT_3D('',#10246,#8417,#8418);
#6563=AXIS2_PLACEMENT_3D('',#10248,#8419,#8420);
#6564=AXIS2_PLACEMENT_3D('',#10249,#8421,#8422);
#6565=AXIS2_PLACEMENT_3D('',#10250,#8423,#8424);
#6566=AXIS2_PLACEMENT_3D('',#10251,#8425,#8426);
#6567=AXIS2_PLACEMENT_3D('',#10254,#8427,#8428);
#6568=AXIS2_PLACEMENT_3D('',#10256,#8429,#8430);
#6569=AXIS2_PLACEMENT_3D('',#10257,#8431,#8432);
#6570=AXIS2_PLACEMENT_3D('',#10258,#8433,#8434);
#6571=AXIS2_PLACEMENT_3D('',#10259,#8435,#8436);
#6572=AXIS2_PLACEMENT_3D('',#10262,#8437,#8438);
#6573=AXIS2_PLACEMENT_3D('',#10264,#8439,#8440);
#6574=AXIS2_PLACEMENT_3D('',#10265,#8441,#8442);
#6575=AXIS2_PLACEMENT_3D('',#10266,#8443,#8444);
#6576=AXIS2_PLACEMENT_3D('',#10269,#8447,#8448);
#6577=AXIS2_PLACEMENT_3D('',#10271,#8449,#8450);
#6578=AXIS2_PLACEMENT_3D('',#10273,#8451,#8452);
#6579=AXIS2_PLACEMENT_3D('',#10275,#8453,#8454);
#6580=AXIS2_PLACEMENT_3D('',#10276,#8455,#8456);
#6581=AXIS2_PLACEMENT_3D('',#10277,#8457,#8458);
#6582=AXIS2_PLACEMENT_3D('',#10280,#8459,#8460);
#6583=AXIS2_PLACEMENT_3D('',#10282,#8461,#8462);
#6584=AXIS2_PLACEMENT_3D('',#10283,#8463,#8464);
#6585=AXIS2_PLACEMENT_3D('',#10284,#8465,#8466);
#6586=AXIS2_PLACEMENT_3D('',#10287,#8469,#8470);
#6587=AXIS2_PLACEMENT_3D('',#10290,#8471,#8472);
#6588=AXIS2_PLACEMENT_3D('',#10292,#8473,#8474);
#6589=AXIS2_PLACEMENT_3D('',#10293,#8475,#8476);
#6590=AXIS2_PLACEMENT_3D('',#10294,#8477,#8478);
#6591=AXIS2_PLACEMENT_3D('',#10297,#8481,#8482);
#6592=AXIS2_PLACEMENT_3D('',#10300,#8483,#8484);
#6593=AXIS2_PLACEMENT_3D('',#10302,#8485,#8486);
#6594=AXIS2_PLACEMENT_3D('',#10303,#8487,#8488);
#6595=AXIS2_PLACEMENT_3D('',#10304,#8489,#8490);
#6596=AXIS2_PLACEMENT_3D('',#10307,#8493,#8494);
#6597=AXIS2_PLACEMENT_3D('',#10310,#8495,#8496);
#6598=AXIS2_PLACEMENT_3D('',#10312,#8497,#8498);
#6599=AXIS2_PLACEMENT_3D('',#10313,#8499,#8500);
#6600=AXIS2_PLACEMENT_3D('',#10314,#8501,#8502);
#6601=AXIS2_PLACEMENT_3D('',#10317,#8505,#8506);
#6602=AXIS2_PLACEMENT_3D('',#10320,#8509,#8510);
#6603=AXIS2_PLACEMENT_3D('',#10323,#8511,#8512);
#6604=AXIS2_PLACEMENT_3D('',#10325,#8513,#8514);
#6605=AXIS2_PLACEMENT_3D('',#10326,#8515,#8516);
#6606=AXIS2_PLACEMENT_3D('',#10327,#8517,#8518);
#6607=AXIS2_PLACEMENT_3D('',#10330,#8519,#8520);
#6608=AXIS2_PLACEMENT_3D('',#10332,#8521,#8522);
#6609=AXIS2_PLACEMENT_3D('',#10333,#8523,#8524);
#6610=AXIS2_PLACEMENT_3D('',#10334,#8525,#8526);
#6611=AXIS2_PLACEMENT_3D('',#10353,#8529,#8530);
#6612=AXIS2_PLACEMENT_3D('',#10356,#8531,#8532);
#6613=AXIS2_PLACEMENT_3D('',#10358,#8533,#8534);
#6614=AXIS2_PLACEMENT_3D('',#10359,#8535,#8536);
#6615=AXIS2_PLACEMENT_3D('',#10360,#8537,#8538);
#6616=AXIS2_PLACEMENT_3D('',#10363,#8541,#8542);
#6617=AXIS2_PLACEMENT_3D('',#10366,#8545,#8546);
#6618=AXIS2_PLACEMENT_3D('',#10385,#8549,#8550);
#6619=AXIS2_PLACEMENT_3D('',#10404,#8553,#8554);
#6620=AXIS2_PLACEMENT_3D('',#10423,#8557,#8558);
#6621=AXIS2_PLACEMENT_3D('',#10426,#8559,#8560);
#6622=AXIS2_PLACEMENT_3D('',#10428,#8561,#8562);
#6623=AXIS2_PLACEMENT_3D('',#10429,#8563,#8564);
#6624=AXIS2_PLACEMENT_3D('',#10430,#8565,#8566);
#6625=AXIS2_PLACEMENT_3D('',#10433,#8567,#8568);
#6626=AXIS2_PLACEMENT_3D('',#10435,#8569,#8570);
#6627=AXIS2_PLACEMENT_3D('',#10436,#8571,#8572);
#6628=AXIS2_PLACEMENT_3D('',#10437,#8573,#8574);
#6629=AXIS2_PLACEMENT_3D('',#10440,#8575,#8576);
#6630=AXIS2_PLACEMENT_3D('',#10442,#8577,#8578);
#6631=AXIS2_PLACEMENT_3D('',#10443,#8579,#8580);
#6632=AXIS2_PLACEMENT_3D('',#10444,#8581,#8582);
#6633=AXIS2_PLACEMENT_3D('',#10447,#8585,#8586);
#6634=AXIS2_PLACEMENT_3D('',#10450,#8587,#8588);
#6635=AXIS2_PLACEMENT_3D('',#10452,#8589,#8590);
#6636=AXIS2_PLACEMENT_3D('',#10453,#8591,#8592);
#6637=AXIS2_PLACEMENT_3D('',#10454,#8593,#8594);
#6638=AXIS2_PLACEMENT_3D('',#10473,#8597,#8598);
#6639=AXIS2_PLACEMENT_3D('',#10476,#8601,#8602);
#6640=AXIS2_PLACEMENT_3D('',#10479,#8605,#8606);
#6641=AXIS2_PLACEMENT_3D('',#10498,#8609,#8610);
#6642=AXIS2_PLACEMENT_3D('',#10501,#8613,#8614);
#6643=AXIS2_PLACEMENT_3D('',#10520,#8617,#8618);
#6644=AXIS2_PLACEMENT_3D('',#10521,#8619,#8620);
#6645=AXIS2_PLACEMENT_3D('',#10522,#8621,#8622);
#6646=AXIS2_PLACEMENT_3D('',#10523,#8623,#8624);
#6647=AXIS2_PLACEMENT_3D('',#10542,#8627,#8628);
#6648=AXIS2_PLACEMENT_3D('',#10543,#8629,#8630);
#6649=AXIS2_PLACEMENT_3D('',#10544,#8631,#8632);
#6650=AXIS2_PLACEMENT_3D('',#10545,#8633,#8634);
#6651=AXIS2_PLACEMENT_3D('',#10546,#8635,#8636);
#6652=AXIS2_PLACEMENT_3D('',#10547,#8637,#8638);
#6653=AXIS2_PLACEMENT_3D('',#10548,#8639,#8640);
#6654=AXIS2_PLACEMENT_3D('',#10549,#8641,#8642);
#6655=AXIS2_PLACEMENT_3D('',#10550,#8643,#8644);
#6656=AXIS2_PLACEMENT_3D('',#10551,#8645,#8646);
#6657=AXIS2_PLACEMENT_3D('',#10554,#8649,#8650);
#6658=AXIS2_PLACEMENT_3D('',#10557,#8653,#8654);
#6659=AXIS2_PLACEMENT_3D('',#10560,#8657,#8658);
#6660=AXIS2_PLACEMENT_3D('',#10563,#8661,#8662);
#6661=AXIS2_PLACEMENT_3D('',#10565,#8664,#8665);
#6662=AXIS2_PLACEMENT_3D('',#10567,#8667,#8668);
#6663=AXIS2_PLACEMENT_3D('',#10569,#8670,#8671);
#6664=AXIS2_PLACEMENT_3D('',#10571,#8673,#8674);
#6665=AXIS2_PLACEMENT_3D('',#10573,#8676,#8677);
#6666=AXIS2_PLACEMENT_3D('',#10576,#8680,#8681);
#6667=AXIS2_PLACEMENT_3D('',#10578,#8683,#8684);
#6668=AXIS2_PLACEMENT_3D('',#10581,#8687,#8688);
#6669=AXIS2_PLACEMENT_3D('',#10583,#8690,#8691);
#6670=AXIS2_PLACEMENT_3D('',#10586,#8694,#8695);
#6671=AXIS2_PLACEMENT_3D('',#10588,#8697,#8698);
#6672=AXIS2_PLACEMENT_3D('',#10590,#8700,#8701);
#6673=AXIS2_PLACEMENT_3D('',#10593,#8704,#8705);
#6674=AXIS2_PLACEMENT_3D('',#10594,#8706,#8707);
#6675=AXIS2_PLACEMENT_3D('',#10595,#8708,#8709);
#6676=AXIS2_PLACEMENT_3D('',#10596,#8710,#8711);
#6677=AXIS2_PLACEMENT_3D('',#10597,#8712,#8713);
#6678=AXIS2_PLACEMENT_3D('',#10598,#8714,#8715);
#6679=AXIS2_PLACEMENT_3D('',#10599,#8716,#8717);
#6680=AXIS2_PLACEMENT_3D('',#10600,#8718,#8719);
#6681=AXIS2_PLACEMENT_3D('',#10601,#8720,#8721);
#6682=AXIS2_PLACEMENT_3D('',#10602,#8722,#8723);
#6683=AXIS2_PLACEMENT_3D('',#10603,#8724,#8725);
#6684=AXIS2_PLACEMENT_3D('',#10604,#8726,#8727);
#6685=AXIS2_PLACEMENT_3D('',#10605,#8728,#8729);
#6686=AXIS2_PLACEMENT_3D('',#10606,#8730,#8731);
#6687=AXIS2_PLACEMENT_3D('',#10607,#8732,#8733);
#6688=AXIS2_PLACEMENT_3D('',#10608,#8734,#8735);
#6689=AXIS2_PLACEMENT_3D('',#10609,#8736,#8737);
#6690=AXIS2_PLACEMENT_3D('',#10610,#8738,#8739);
#6691=AXIS2_PLACEMENT_3D('',#10611,#8740,#8741);
#6692=AXIS2_PLACEMENT_3D('',#10612,#8742,#8743);
#6693=AXIS2_PLACEMENT_3D('',#10613,#8744,#8745);
#6694=AXIS2_PLACEMENT_3D('',#10614,#8746,#8747);
#6695=AXIS2_PLACEMENT_3D('',#10615,#8748,#8749);
#6696=DIRECTION('axis',(0.,0.,1.));
#6697=DIRECTION('refdir',(1.,0.,0.));
#6698=DIRECTION('axis',(0.,0.,1.));
#6699=DIRECTION('refdir',(1.,0.,0.));
#6700=DIRECTION('center_axis',(-1.,0.,0.));
#6701=DIRECTION('ref_axis',(0.,1.,0.));
#6702=DIRECTION('center_axis',(-1.,0.,0.));
#6703=DIRECTION('ref_axis',(0.,1.,0.));
#6704=DIRECTION('',(-1.,0.,0.));
#6705=DIRECTION('center_axis',(1.,0.,0.));
#6706=DIRECTION('ref_axis',(0.,1.,0.));
#6707=DIRECTION('center_axis',(0.,-1.,0.));
#6708=DIRECTION('ref_axis',(-1.,0.,0.));
#6709=DIRECTION('',(1.,0.,0.));
#6710=DIRECTION('',(0.,0.,-1.));
#6711=DIRECTION('',(-1.,0.,0.));
#6712=DIRECTION('',(0.,0.,-1.));
#6713=DIRECTION('center_axis',(1.,0.,0.));
#6714=DIRECTION('ref_axis',(0.,-1.,0.));
#6715=DIRECTION('',(0.,1.,0.));
#6716=DIRECTION('',(0.,-1.,0.));
#6717=DIRECTION('',(0.,0.,-1.));
#6718=DIRECTION('center_axis',(0.,1.,0.));
#6719=DIRECTION('ref_axis',(1.,0.,0.));
#6720=DIRECTION('',(-1.,0.,0.));
#6721=DIRECTION('',(1.,0.,0.));
#6722=DIRECTION('',(0.,0.,-1.));
#6723=DIRECTION('center_axis',(-1.,0.,0.));
#6724=DIRECTION('ref_axis',(0.,1.,0.));
#6725=DIRECTION('',(0.,-1.,0.));
#6726=DIRECTION('',(0.,1.,0.));
#6727=DIRECTION('center_axis',(0.,0.,-1.));
#6728=DIRECTION('ref_axis',(-1.,0.,0.));
#6729=DIRECTION('center_axis',(-1.,0.,0.));
#6730=DIRECTION('ref_axis',(0.,0.,1.));
#6731=DIRECTION('center_axis',(1.,0.,0.));
#6732=DIRECTION('ref_axis',(0.,1.,0.));
#6733=DIRECTION('center_axis',(0.,-1.,0.));
#6734=DIRECTION('ref_axis',(0.,0.,-1.));
#6735=DIRECTION('center_axis',(-1.,0.,0.));
#6736=DIRECTION('ref_axis',(0.,1.,0.));
#6737=DIRECTION('center_axis',(-1.,0.,0.));
#6738=DIRECTION('ref_axis',(0.,1.,0.));
#6739=DIRECTION('center_axis',(1.,0.,0.));
#6740=DIRECTION('ref_axis',(0.,0.,-1.));
#6741=DIRECTION('',(0.,0.,1.));
#6742=DIRECTION('',(0.,-1.,0.));
#6743=DIRECTION('center_axis',(1.,0.,0.));
#6744=DIRECTION('ref_axis',(0.,0.707106781186545,0.70710678118655));
#6745=DIRECTION('',(0.,0.,1.));
#6746=DIRECTION('',(0.,-1.,0.));
#6747=DIRECTION('center_axis',(1.,0.,0.));
#6748=DIRECTION('ref_axis',(0.,0.707106781186545,0.70710678118655));
#6749=DIRECTION('',(0.,0.,1.));
#6750=DIRECTION('',(0.,-1.,0.));
#6751=DIRECTION('',(0.,0.,-1.));
#6752=DIRECTION('',(0.,-1.,0.));
#6753=DIRECTION('',(0.,0.,-1.));
#6754=DIRECTION('',(0.,-1.,0.));
#6755=DIRECTION('',(0.,0.,1.));
#6756=DIRECTION('',(0.,-1.,0.));
#6757=DIRECTION('',(0.,0.,1.));
#6758=DIRECTION('',(0.,-1.,0.));
#6759=DIRECTION('',(0.,0.,-1.));
#6760=DIRECTION('center_axis',(1.,0.,0.));
#6761=DIRECTION('ref_axis',(0.,-0.707106781186545,0.70710678118655));
#6762=DIRECTION('',(0.,-1.,0.));
#6763=DIRECTION('',(0.,0.,-1.));
#6764=DIRECTION('center_axis',(1.,0.,0.));
#6765=DIRECTION('ref_axis',(0.,-0.70710678118655,0.707106781186545));
#6766=DIRECTION('',(0.,-1.,0.));
#6767=DIRECTION('',(0.,0.,-1.));
#6768=DIRECTION('',(0.,1.,0.));
#6769=DIRECTION('center_axis',(1.,0.,0.));
#6770=DIRECTION('ref_axis',(0.,-1.,0.));
#6771=DIRECTION('center_axis',(1.,0.,0.));
#6772=DIRECTION('ref_axis',(0.,1.,0.));
#6773=DIRECTION('',(-1.,0.,0.));
#6774=DIRECTION('center_axis',(1.,0.,0.));
#6775=DIRECTION('ref_axis',(0.,1.,0.));
#6776=DIRECTION('center_axis',(1.,0.,0.));
#6777=DIRECTION('ref_axis',(0.,1.,0.));
#6778=DIRECTION('center_axis',(1.,0.,0.));
#6779=DIRECTION('ref_axis',(0.,0.,-1.));
#6780=DIRECTION('center_axis',(-1.,0.,0.));
#6781=DIRECTION('ref_axis',(0.,-1.,0.));
#6782=DIRECTION('center_axis',(0.,-1.,0.));
#6783=DIRECTION('ref_axis',(0.,0.,1.));
#6784=DIRECTION('center_axis',(-1.,0.,0.));
#6785=DIRECTION('ref_axis',(0.,-1.,0.));
#6786=DIRECTION('center_axis',(-1.,0.,0.));
#6787=DIRECTION('ref_axis',(0.,-1.,0.));
#6788=DIRECTION('',(-1.,0.,0.));
#6789=DIRECTION('center_axis',(1.,0.,0.));
#6790=DIRECTION('ref_axis',(0.,-1.,0.));
#6791=DIRECTION('center_axis',(1.,0.,0.));
#6792=DIRECTION('ref_axis',(0.,-1.,0.));
#6793=DIRECTION('center_axis',(1.,0.,0.));
#6794=DIRECTION('ref_axis',(0.,0.,-1.));
#6795=DIRECTION('center_axis',(-1.,0.,0.));
#6796=DIRECTION('ref_axis',(0.,1.,0.));
#6797=DIRECTION('center_axis',(0.,-1.,0.));
#6798=DIRECTION('ref_axis',(0.,0.,1.));
#6799=DIRECTION('center_axis',(-1.,0.,0.));
#6800=DIRECTION('ref_axis',(0.,0.,1.));
#6801=DIRECTION('center_axis',(-1.,0.,0.));
#6802=DIRECTION('ref_axis',(0.,0.707106781186545,0.70710678118655));
#6803=DIRECTION('',(0.,1.,0.));
#6804=DIRECTION('',(0.,0.,-1.));
#6805=DIRECTION('',(0.,-1.,0.));
#6806=DIRECTION('',(0.,0.,1.));
#6807=DIRECTION('',(0.,1.,0.));
#6808=DIRECTION('center_axis',(-1.,0.,0.));
#6809=DIRECTION('ref_axis',(0.,-0.70710678118655,0.707106781186545));
#6810=DIRECTION('',(0.,0.,1.));
#6811=DIRECTION('',(0.,1.,0.));
#6812=DIRECTION('center_axis',(-1.,0.,0.));
#6813=DIRECTION('ref_axis',(0.,-0.707106781186545,0.70710678118655));
#6814=DIRECTION('',(0.,0.,1.));
#6815=DIRECTION('',(0.,1.,0.));
#6816=DIRECTION('',(0.,0.,-1.));
#6817=DIRECTION('',(0.,1.,0.));
#6818=DIRECTION('',(0.,0.,-1.));
#6819=DIRECTION('',(0.,1.,0.));
#6820=DIRECTION('',(0.,0.,1.));
#6821=DIRECTION('',(0.,1.,0.));
#6822=DIRECTION('',(0.,0.,1.));
#6823=DIRECTION('',(0.,1.,0.));
#6824=DIRECTION('',(0.,0.,-1.));
#6825=DIRECTION('center_axis',(-1.,0.,0.));
#6826=DIRECTION('ref_axis',(0.,0.707106781186545,0.70710678118655));
#6827=DIRECTION('',(0.,1.,0.));
#6828=DIRECTION('',(0.,0.,-1.));
#6829=DIRECTION('center_axis',(-1.,0.,0.));
#6830=DIRECTION('ref_axis',(0.,-1.,0.));
#6831=DIRECTION('center_axis',(-1.,0.,0.));
#6832=DIRECTION('ref_axis',(0.,0.,1.));
#6833=DIRECTION('center_axis',(0.,-1.,0.));
#6834=DIRECTION('ref_axis',(0.,0.,-1.));
#6835=DIRECTION('center_axis',(0.,0.,-1.));
#6836=DIRECTION('ref_axis',(-1.,0.,0.));
#6837=DIRECTION('center_axis',(0.,0.,1.));
#6838=DIRECTION('ref_axis',(-1.,0.,0.));
#6839=DIRECTION('center_axis',(0.,-1.,0.));
#6840=DIRECTION('ref_axis',(1.,0.,0.));
#6841=DIRECTION('center_axis',(0.,0.,-1.));
#6842=DIRECTION('ref_axis',(-1.,0.,0.));
#6843=DIRECTION('center_axis',(0.,0.,1.));
#6844=DIRECTION('ref_axis',(0.,-1.,0.));
#6845=DIRECTION('',(-1.,0.,0.));
#6846=DIRECTION('',(0.,-1.,0.));
#6847=DIRECTION('',(1.,0.,0.));
#6848=DIRECTION('',(0.,1.,0.));
#6849=DIRECTION('center_axis',(0.,0.,1.));
#6850=DIRECTION('ref_axis',(-1.,0.,0.));
#6851=DIRECTION('center_axis',(0.,0.,1.));
#6852=DIRECTION('ref_axis',(-1.,0.,0.));
#6853=DIRECTION('center_axis',(0.,0.,1.));
#6854=DIRECTION('ref_axis',(-1.,0.,0.));
#6855=DIRECTION('center_axis',(0.,0.,1.));
#6856=DIRECTION('ref_axis',(0.,1.,0.));
#6857=DIRECTION('center_axis',(0.,0.,1.));
#6858=DIRECTION('ref_axis',(0.,1.,0.));
#6859=DIRECTION('center_axis',(0.,0.,1.));
#6860=DIRECTION('ref_axis',(-1.,0.,0.));
#6861=DIRECTION('center_axis',(0.,0.,1.));
#6862=DIRECTION('ref_axis',(-1.,0.,0.));
#6863=DIRECTION('center_axis',(0.,0.,1.));
#6864=DIRECTION('ref_axis',(-1.,0.,0.));
#6865=DIRECTION('center_axis',(0.,0.,1.));
#6866=DIRECTION('ref_axis',(-1.,0.,0.));
#6867=DIRECTION('center_axis',(0.,0.,1.));
#6868=DIRECTION('ref_axis',(-1.,0.,0.));
#6869=DIRECTION('center_axis',(0.,0.,1.));
#6870=DIRECTION('ref_axis',(-1.,0.,0.));
#6871=DIRECTION('center_axis',(0.,0.,1.));
#6872=DIRECTION('ref_axis',(-1.,0.,0.));
#6873=DIRECTION('center_axis',(0.,0.,1.));
#6874=DIRECTION('ref_axis',(-1.,0.,0.));
#6875=DIRECTION('center_axis',(0.,0.,1.));
#6876=DIRECTION('ref_axis',(-1.,0.,0.));
#6877=DIRECTION('center_axis',(0.,0.,1.));
#6878=DIRECTION('ref_axis',(-1.,0.,0.));
#6879=DIRECTION('center_axis',(0.,0.,-1.));
#6880=DIRECTION('ref_axis',(-1.,0.,0.));
#6881=DIRECTION('',(0.,0.,-1.));
#6882=DIRECTION('center_axis',(0.,0.,-1.));
#6883=DIRECTION('ref_axis',(-1.,0.,0.));
#6884=DIRECTION('center_axis',(0.,0.,-1.));
#6885=DIRECTION('ref_axis',(-1.,0.,0.));
#6886=DIRECTION('center_axis',(0.,-1.,0.));
#6887=DIRECTION('ref_axis',(1.,0.,0.));
#6888=DIRECTION('center_axis',(0.,0.,-1.));
#6889=DIRECTION('ref_axis',(-1.,0.,0.));
#6890=DIRECTION('center_axis',(0.,0.,-1.));
#6891=DIRECTION('ref_axis',(-1.,0.,0.));
#6892=DIRECTION('',(0.,0.,-1.));
#6893=DIRECTION('center_axis',(0.,0.,-1.));
#6894=DIRECTION('ref_axis',(-1.,0.,0.));
#6895=DIRECTION('center_axis',(0.,0.,-1.));
#6896=DIRECTION('ref_axis',(-1.,0.,0.));
#6897=DIRECTION('center_axis',(0.,-1.,0.));
#6898=DIRECTION('ref_axis',(1.,0.,0.));
#6899=DIRECTION('center_axis',(0.,0.,-1.));
#6900=DIRECTION('ref_axis',(-1.,0.,0.));
#6901=DIRECTION('center_axis',(0.,0.,-1.));
#6902=DIRECTION('ref_axis',(-1.,0.,0.));
#6903=DIRECTION('',(0.,0.,-1.));
#6904=DIRECTION('center_axis',(0.,0.,-1.));
#6905=DIRECTION('ref_axis',(-1.,0.,0.));
#6906=DIRECTION('center_axis',(0.,0.,-1.));
#6907=DIRECTION('ref_axis',(-1.,0.,0.));
#6908=DIRECTION('center_axis',(0.,-1.,0.));
#6909=DIRECTION('ref_axis',(1.,0.,0.));
#6910=DIRECTION('center_axis',(0.,0.,-1.));
#6911=DIRECTION('ref_axis',(-1.,0.,0.));
#6912=DIRECTION('center_axis',(0.,0.,-1.));
#6913=DIRECTION('ref_axis',(-1.,0.,0.));
#6914=DIRECTION('',(0.,0.,-1.));
#6915=DIRECTION('center_axis',(0.,0.,-1.));
#6916=DIRECTION('ref_axis',(-1.,0.,0.));
#6917=DIRECTION('center_axis',(0.,0.,-1.));
#6918=DIRECTION('ref_axis',(-1.,0.,0.));
#6919=DIRECTION('center_axis',(0.,-1.,0.));
#6920=DIRECTION('ref_axis',(1.,0.,0.));
#6921=DIRECTION('center_axis',(0.,0.,-1.));
#6922=DIRECTION('ref_axis',(-1.,0.,0.));
#6923=DIRECTION('center_axis',(0.,0.,-1.));
#6924=DIRECTION('ref_axis',(-1.,0.,0.));
#6925=DIRECTION('',(0.,0.,-1.));
#6926=DIRECTION('center_axis',(0.,0.,-1.));
#6927=DIRECTION('ref_axis',(-1.,0.,0.));
#6928=DIRECTION('center_axis',(0.,0.,-1.));
#6929=DIRECTION('ref_axis',(-1.,0.,0.));
#6930=DIRECTION('center_axis',(0.,-1.,0.));
#6931=DIRECTION('ref_axis',(1.,0.,0.));
#6932=DIRECTION('center_axis',(0.,0.,-1.));
#6933=DIRECTION('ref_axis',(-1.,0.,0.));
#6934=DIRECTION('center_axis',(0.,0.,-1.));
#6935=DIRECTION('ref_axis',(-1.,0.,0.));
#6936=DIRECTION('',(0.,0.,-1.));
#6937=DIRECTION('center_axis',(0.,0.,-1.));
#6938=DIRECTION('ref_axis',(-1.,0.,0.));
#6939=DIRECTION('center_axis',(0.,0.,-1.));
#6940=DIRECTION('ref_axis',(-1.,0.,0.));
#6941=DIRECTION('center_axis',(0.,-1.,0.));
#6942=DIRECTION('ref_axis',(1.,0.,0.));
#6943=DIRECTION('center_axis',(0.,0.,-1.));
#6944=DIRECTION('ref_axis',(-1.,0.,0.));
#6945=DIRECTION('center_axis',(0.,0.,-1.));
#6946=DIRECTION('ref_axis',(-1.,0.,0.));
#6947=DIRECTION('',(0.,0.,-1.));
#6948=DIRECTION('center_axis',(0.,0.,-1.));
#6949=DIRECTION('ref_axis',(-1.,0.,0.));
#6950=DIRECTION('center_axis',(0.,0.,-1.));
#6951=DIRECTION('ref_axis',(-1.,0.,0.));
#6952=DIRECTION('center_axis',(0.,-1.,0.));
#6953=DIRECTION('ref_axis',(1.,0.,0.));
#6954=DIRECTION('center_axis',(0.,0.,-1.));
#6955=DIRECTION('ref_axis',(0.,1.,0.));
#6956=DIRECTION('center_axis',(0.,0.,-1.));
#6957=DIRECTION('ref_axis',(0.,1.,0.));
#6958=DIRECTION('center_axis',(0.,0.,-1.));
#6959=DIRECTION('ref_axis',(0.,1.,0.));
#6960=DIRECTION('',(0.,0.,-1.));
#6961=DIRECTION('center_axis',(0.,0.,-1.));
#6962=DIRECTION('ref_axis',(0.,1.,0.));
#6963=DIRECTION('center_axis',(0.,0.,-1.));
#6964=DIRECTION('ref_axis',(-1.,0.,0.));
#6965=DIRECTION('center_axis',(0.,-1.,0.));
#6966=DIRECTION('ref_axis',(1.,0.,0.));
#6967=DIRECTION('center_axis',(0.,0.,-1.));
#6968=DIRECTION('ref_axis',(-1.,0.,0.));
#6969=DIRECTION('center_axis',(0.,0.,-1.));
#6970=DIRECTION('ref_axis',(-1.,0.,0.));
#6971=DIRECTION('',(0.,0.,-1.));
#6972=DIRECTION('center_axis',(0.,0.,-1.));
#6973=DIRECTION('ref_axis',(-1.,0.,0.));
#6974=DIRECTION('center_axis',(0.,0.,-1.));
#6975=DIRECTION('ref_axis',(-1.,0.,0.));
#6976=DIRECTION('center_axis',(0.,-1.,0.));
#6977=DIRECTION('ref_axis',(1.,0.,0.));
#6978=DIRECTION('center_axis',(0.,0.,-1.));
#6979=DIRECTION('ref_axis',(0.,1.,0.));
#6980=DIRECTION('center_axis',(0.,0.,-1.));
#6981=DIRECTION('ref_axis',(0.,1.,0.));
#6982=DIRECTION('center_axis',(0.,0.,-1.));
#6983=DIRECTION('ref_axis',(0.,1.,0.));
#6984=DIRECTION('',(0.,0.,-1.));
#6985=DIRECTION('center_axis',(0.,0.,-1.));
#6986=DIRECTION('ref_axis',(0.,1.,0.));
#6987=DIRECTION('center_axis',(0.,0.,-1.));
#6988=DIRECTION('ref_axis',(-1.,0.,0.));
#6989=DIRECTION('center_axis',(0.,-1.,0.));
#6990=DIRECTION('ref_axis',(1.,0.,0.));
#6991=DIRECTION('center_axis',(0.,0.,-1.));
#6992=DIRECTION('ref_axis',(-1.,0.,0.));
#6993=DIRECTION('center_axis',(0.,0.,-1.));
#6994=DIRECTION('ref_axis',(-1.,0.,0.));
#6995=DIRECTION('',(0.,0.,-1.));
#6996=DIRECTION('center_axis',(0.,0.,-1.));
#6997=DIRECTION('ref_axis',(-1.,0.,0.));
#6998=DIRECTION('center_axis',(0.,0.,-1.));
#6999=DIRECTION('ref_axis',(-1.,0.,0.));
#7000=DIRECTION('center_axis',(0.,-1.,0.));
#7001=DIRECTION('ref_axis',(1.,0.,0.));
#7002=DIRECTION('center_axis',(0.,0.,-1.));
#7003=DIRECTION('ref_axis',(-1.,0.,0.));
#7004=DIRECTION('center_axis',(0.,0.,-1.));
#7005=DIRECTION('ref_axis',(-1.,0.,0.));
#7006=DIRECTION('',(0.,0.,-1.));
#7007=DIRECTION('center_axis',(0.,0.,-1.));
#7008=DIRECTION('ref_axis',(-1.,0.,0.));
#7009=DIRECTION('center_axis',(0.,0.,-1.));
#7010=DIRECTION('ref_axis',(-1.,0.,0.));
#7011=DIRECTION('center_axis',(0.,-1.,0.));
#7012=DIRECTION('ref_axis',(1.,0.,0.));
#7013=DIRECTION('center_axis',(0.,0.,-1.));
#7014=DIRECTION('ref_axis',(-1.,0.,0.));
#7015=DIRECTION('center_axis',(0.,0.,-1.));
#7016=DIRECTION('ref_axis',(-1.,0.,0.));
#7017=DIRECTION('',(0.,0.,-1.));
#7018=DIRECTION('center_axis',(0.,0.,-1.));
#7019=DIRECTION('ref_axis',(-1.,0.,0.));
#7020=DIRECTION('center_axis',(0.,0.,-1.));
#7021=DIRECTION('ref_axis',(-1.,0.,0.));
#7022=DIRECTION('center_axis',(0.,-1.,0.));
#7023=DIRECTION('ref_axis',(1.,0.,0.));
#7024=DIRECTION('center_axis',(0.,0.,-1.));
#7025=DIRECTION('ref_axis',(-1.,0.,0.));
#7026=DIRECTION('center_axis',(0.,0.,-1.));
#7027=DIRECTION('ref_axis',(-1.,0.,0.));
#7028=DIRECTION('',(0.,0.,-1.));
#7029=DIRECTION('center_axis',(0.,0.,-1.));
#7030=DIRECTION('ref_axis',(-1.,0.,0.));
#7031=DIRECTION('center_axis',(0.,0.,-1.));
#7032=DIRECTION('ref_axis',(-1.,0.,0.));
#7033=DIRECTION('center_axis',(0.,-1.,0.));
#7034=DIRECTION('ref_axis',(1.,0.,0.));
#7035=DIRECTION('center_axis',(0.,0.,-1.));
#7036=DIRECTION('ref_axis',(-1.,0.,0.));
#7037=DIRECTION('center_axis',(0.,0.,-1.));
#7038=DIRECTION('ref_axis',(-1.,0.,0.));
#7039=DIRECTION('',(0.,0.,-1.));
#7040=DIRECTION('center_axis',(0.,0.,-1.));
#7041=DIRECTION('ref_axis',(-1.,0.,0.));
#7042=DIRECTION('center_axis',(0.,0.,-1.));
#7043=DIRECTION('ref_axis',(-1.,0.,0.));
#7044=DIRECTION('center_axis',(0.,-1.,0.));
#7045=DIRECTION('ref_axis',(1.,0.,0.));
#7046=DIRECTION('center_axis',(0.,0.,-1.));
#7047=DIRECTION('ref_axis',(-1.,0.,0.));
#7048=DIRECTION('center_axis',(0.,0.,-1.));
#7049=DIRECTION('ref_axis',(-1.,0.,0.));
#7050=DIRECTION('',(0.,0.,-1.));
#7051=DIRECTION('center_axis',(0.,0.,-1.));
#7052=DIRECTION('ref_axis',(-1.,0.,0.));
#7053=DIRECTION('center_axis',(0.,1.,0.));
#7054=DIRECTION('ref_axis',(0.70710678118655,0.,-0.707106781186545));
#7055=DIRECTION('center_axis',(0.,0.707106781186545,0.70710678118655));
#7056=DIRECTION('ref_axis',(0.,-0.70710678118655,0.707106781186545));
#7057=DIRECTION('',(0.,1.,0.));
#7058=DIRECTION('center_axis',(0.,0.707106781186545,-0.70710678118655));
#7059=DIRECTION('ref_axis',(0.,0.70710678118655,0.707106781186545));
#7060=DIRECTION('center_axis',(0.,-1.,0.));
#7061=DIRECTION('ref_axis',(-0.70710678118655,0.,-0.707106781186545));
#7062=DIRECTION('center_axis',(0.,-0.707106781186545,0.70710678118655));
#7063=DIRECTION('ref_axis',(0.,0.70710678118655,0.707106781186545));
#7064=DIRECTION('',(0.,-1.,0.));
#7065=DIRECTION('center_axis',(0.,-0.707106781186545,-0.70710678118655));
#7066=DIRECTION('ref_axis',(0.,0.70710678118655,-0.707106781186545));
#7067=DIRECTION('center_axis',(0.,0.,1.));
#7068=DIRECTION('ref_axis',(-0.707106781186553,-0.707106781186542,0.));
#7069=DIRECTION('center_axis',(0.,-0.707106781186548,0.707106781186548));
#7070=DIRECTION('ref_axis',(0.,-0.707106781186547,-0.707106781186547));
#7071=DIRECTION('',(0.,0.,1.));
#7072=DIRECTION('center_axis',(0.,0.,-1.));
#7073=DIRECTION('ref_axis',(0.707106781186553,0.707106781186542,0.));
#7074=DIRECTION('center_axis',(0.,0.707106781186548,0.707106781186548));
#7075=DIRECTION('ref_axis',(0.,-0.707106781186547,0.707106781186547));
#7076=DIRECTION('',(0.,0.,1.));
#7077=DIRECTION('center_axis',(0.,-1.,0.));
#7078=DIRECTION('ref_axis',(-0.70710678118655,0.,-0.707106781186545));
#7079=DIRECTION('center_axis',(0.,-0.707106781186548,0.707106781186548));
#7080=DIRECTION('ref_axis',(0.,0.707106781186548,0.707106781186548));
#7081=DIRECTION('',(0.,-1.,0.));
#7082=DIRECTION('center_axis',(0.,-1.,0.));
#7083=DIRECTION('ref_axis',(0.70710678118655,0.,-0.707106781186545));
#7084=DIRECTION('center_axis',(0.,0.707106781186548,0.707106781186548));
#7085=DIRECTION('ref_axis',(0.,0.707106781186548,-0.707106781186548));
#7086=DIRECTION('',(0.,1.,0.));
#7087=DIRECTION('center_axis',(0.,1.,0.));
#7088=DIRECTION('ref_axis',(-0.70710678118655,0.,-0.707106781186545));
#7089=DIRECTION('',(0.,-1.,0.));
#7090=DIRECTION('center_axis',(0.,0.707106781186548,0.707106781186548));
#7091=DIRECTION('ref_axis',(0.,-0.707106781186548,0.707106781186548));
#7092=DIRECTION('center_axis',(0.,-0.707106781186548,-0.707106781186548));
#7093=DIRECTION('ref_axis',(0.,-0.707106781186548,0.707106781186548));
#7094=DIRECTION('center_axis',(0.,0.,1.));
#7095=DIRECTION('ref_axis',(-0.707106781186553,-0.707106781186542,0.));
#7096=DIRECTION('center_axis',(0.,-0.707106781186548,0.707106781186548));
#7097=DIRECTION('ref_axis',(0.,-0.707106781186547,-0.707106781186547));
#7098=DIRECTION('',(0.,0.,1.));
#7099=DIRECTION('center_axis',(0.408248290463863,-0.816496580927726,-0.408248290463863));
#7100=DIRECTION('ref_axis',(0.577350269189625,0.577350269189625,-0.577350269189628));
#7101=DIRECTION('center_axis',(0.,1.,0.));
#7102=DIRECTION('ref_axis',(0.,0.,-1.));
#7103=DIRECTION('center_axis',(1.,0.,0.));
#7104=DIRECTION('ref_axis',(0.,1.,0.));
#7105=DIRECTION('center_axis',(0.,0.,-1.));
#7106=DIRECTION('ref_axis',(1.,0.,0.));
#7107=DIRECTION('center_axis',(-0.408248290463859,-0.816496580927729,-0.408248290463862));
#7108=DIRECTION('ref_axis',(-0.577350269189624,0.577350269189624,-0.57735026918963));
#7109=DIRECTION('center_axis',(0.,0.,-1.));
#7110=DIRECTION('ref_axis',(0.,1.,0.));
#7111=DIRECTION('center_axis',(-1.,0.,0.));
#7112=DIRECTION('ref_axis',(0.,0.,-1.));
#7113=DIRECTION('center_axis',(0.,1.,0.));
#7114=DIRECTION('ref_axis',(-1.,0.,0.));
#7115=DIRECTION('center_axis',(1.,0.,0.));
#7116=DIRECTION('ref_axis',(0.,0.70710678118654,-0.707106781186555));
#7117=DIRECTION('',(-1.,0.,0.));
#7118=DIRECTION('',(1.,0.,0.));
#7119=DIRECTION('center_axis',(0.,-1.,0.));
#7120=DIRECTION('ref_axis',(-0.70710678118655,0.,-0.707106781186545));
#7121=DIRECTION('',(0.,-1.,0.));
#7122=DIRECTION('center_axis',(-0.408248290463863,-0.816496580927726,0.408248290463863));
#7123=DIRECTION('ref_axis',(0.577350269189625,-0.577350269189625,-0.577350269189628));
#7124=DIRECTION('center_axis',(1.,0.,0.));
#7125=DIRECTION('ref_axis',(0.,0.,-1.));
#7126=DIRECTION('center_axis',(0.,-1.,0.));
#7127=DIRECTION('ref_axis',(1.,0.,0.));
#7128=DIRECTION('center_axis',(0.,0.,-1.));
#7129=DIRECTION('ref_axis',(0.,-1.,0.));
#7130=DIRECTION('center_axis',(0.,-1.,0.));
#7131=DIRECTION('ref_axis',(0.70710678118655,0.,-0.707106781186545));
#7132=DIRECTION('',(0.,1.,0.));
#7133=DIRECTION('center_axis',(0.,-0.707106781186548,-0.707106781186548));
#7134=DIRECTION('ref_axis',(0.,0.707106781186548,-0.707106781186548));
#7135=DIRECTION('center_axis',(-1.,0.,0.));
#7136=DIRECTION('ref_axis',(0.,0.,1.));
#7137=DIRECTION('center_axis',(-1.,0.,0.));
#7138=DIRECTION('ref_axis',(0.,0.,1.));
#7139=DIRECTION('center_axis',(0.,1.,0.));
#7140=DIRECTION('ref_axis',(1.,0.,0.));
#7141=DIRECTION('center_axis',(0.,0.,-1.));
#7142=DIRECTION('ref_axis',(0.,1.,0.));
#7143=DIRECTION('center_axis',(0.408248290463859,-0.816496580927729,0.408248290463862));
#7144=DIRECTION('ref_axis',(-0.577350269189624,-0.577350269189624,-0.57735026918963));
#7145=DIRECTION('center_axis',(0.,0.,-1.));
#7146=DIRECTION('ref_axis',(-1.,0.,0.));
#7147=DIRECTION('center_axis',(0.,-1.,0.));
#7148=DIRECTION('ref_axis',(0.,0.,-1.));
#7149=DIRECTION('center_axis',(-1.,0.,0.));
#7150=DIRECTION('ref_axis',(0.,-1.,0.));
#7151=DIRECTION('center_axis',(0.,1.,0.));
#7152=DIRECTION('ref_axis',(-0.70710678118655,0.,-0.707106781186545));
#7153=DIRECTION('',(0.,-1.,0.));
#7154=DIRECTION('center_axis',(0.,-0.707106781186548,-0.707106781186548));
#7155=DIRECTION('ref_axis',(0.,-0.707106781186548,0.707106781186548));
#7156=DIRECTION('center_axis',(1.,0.,0.));
#7157=DIRECTION('ref_axis',(0.,-0.70710678118654,-0.707106781186555));
#7158=DIRECTION('',(-1.,0.,0.));
#7159=DIRECTION('',(1.,0.,0.));
#7160=DIRECTION('center_axis',(1.,0.,0.));
#7161=DIRECTION('ref_axis',(0.,0.,-1.));
#7162=DIRECTION('center_axis',(1.,0.,0.));
#7163=DIRECTION('ref_axis',(0.,-1.,0.));
#7164=DIRECTION('center_axis',(0.,0.,-1.));
#7165=DIRECTION('ref_axis',(-1.,0.,0.));
#7166=DIRECTION('center_axis',(0.,1.,0.));
#7167=DIRECTION('ref_axis',(0.,0.,-1.));
#7168=DIRECTION('center_axis',(0.,0.,-1.));
#7169=DIRECTION('ref_axis',(-0.707106781186558,0.707106781186537,0.));
#7170=DIRECTION('',(0.,0.,-1.));
#7171=DIRECTION('center_axis',(1.,0.,0.));
#7172=DIRECTION('ref_axis',(0.,0.,-1.));
#7173=DIRECTION('center_axis',(0.,-1.,0.));
#7174=DIRECTION('ref_axis',(0.,0.,-1.));
#7175=DIRECTION('center_axis',(-1.,0.,0.));
#7176=DIRECTION('ref_axis',(0.,1.,0.));
#7177=DIRECTION('center_axis',(0.,0.,-1.));
#7178=DIRECTION('ref_axis',(1.,0.,0.));
#7179=DIRECTION('center_axis',(0.408248290463863,-0.816496580927726,-0.408248290463863));
#7180=DIRECTION('ref_axis',(0.577350269189625,0.577350269189625,-0.577350269189628));
#7181=DIRECTION('center_axis',(0.,1.,0.));
#7182=DIRECTION('ref_axis',(0.,0.,-1.));
#7183=DIRECTION('center_axis',(1.,0.,0.));
#7184=DIRECTION('ref_axis',(0.,1.,0.));
#7185=DIRECTION('center_axis',(0.,0.,-1.));
#7186=DIRECTION('ref_axis',(1.,0.,0.));
#7187=DIRECTION('center_axis',(1.,0.,0.));
#7188=DIRECTION('ref_axis',(0.,0.,-1.));
#7189=DIRECTION('center_axis',(1.,0.,0.));
#7190=DIRECTION('ref_axis',(0.,0.,1.));
#7191=DIRECTION('center_axis',(0.,-1.,0.));
#7192=DIRECTION('ref_axis',(-1.,0.,0.));
#7193=DIRECTION('center_axis',(0.,0.,-1.));
#7194=DIRECTION('ref_axis',(0.,-1.,0.));
#7195=DIRECTION('center_axis',(-0.408248290463859,-0.816496580927729,-0.408248290463862));
#7196=DIRECTION('ref_axis',(-0.577350269189624,0.577350269189624,-0.57735026918963));
#7197=DIRECTION('center_axis',(0.,0.,-1.));
#7198=DIRECTION('ref_axis',(0.,1.,0.));
#7199=DIRECTION('center_axis',(-1.,0.,0.));
#7200=DIRECTION('ref_axis',(0.,0.,-1.));
#7201=DIRECTION('center_axis',(0.,1.,0.));
#7202=DIRECTION('ref_axis',(-1.,0.,0.));
#7203=DIRECTION('center_axis',(1.,0.,0.));
#7204=DIRECTION('ref_axis',(0.,0.70710678118655,-0.707106781186545));
#7205=DIRECTION('',(-1.,0.,0.));
#7206=DIRECTION('',(1.,0.,0.));
#7207=DIRECTION('center_axis',(0.,-1.,0.));
#7208=DIRECTION('ref_axis',(-0.70710678118655,0.,-0.707106781186545));
#7209=DIRECTION('',(0.,-1.,0.));
#7210=DIRECTION('center_axis',(-0.40824829046385,-0.816496580927735,0.408248290463859));
#7211=DIRECTION('ref_axis',(0.577350269189634,-0.57735026918961,-0.577350269189634));
#7212=DIRECTION('center_axis',(0.,0.,-1.));
#7213=DIRECTION('ref_axis',(0.,-1.,0.));
#7214=DIRECTION('center_axis',(1.,0.,0.));
#7215=DIRECTION('ref_axis',(0.,0.,-1.));
#7216=DIRECTION('center_axis',(0.,-1.,1.48029736616687E-14));
#7217=DIRECTION('ref_axis',(1.,0.,0.));
#7218=DIRECTION('center_axis',(-1.,0.,0.));
#7219=DIRECTION('ref_axis',(0.,0.,1.));
#7220=DIRECTION('center_axis',(-1.,0.,0.));
#7221=DIRECTION('ref_axis',(0.,0.,1.));
#7222=DIRECTION('center_axis',(0.,1.,0.));
#7223=DIRECTION('ref_axis',(1.,0.,0.));
#7224=DIRECTION('center_axis',(0.,0.,-1.));
#7225=DIRECTION('ref_axis',(0.,1.,0.));
#7226=DIRECTION('center_axis',(0.408248290463855,-0.816496580927734,0.408248290463855));
#7227=DIRECTION('ref_axis',(-0.577350269189634,-0.57735026918961,-0.577350269189634));
#7228=DIRECTION('center_axis',(-1.48029736616688E-14,-1.,0.));
#7229=DIRECTION('ref_axis',(0.,0.,-1.));
#7230=DIRECTION('center_axis',(-1.,0.,0.));
#7231=DIRECTION('ref_axis',(0.,-1.,0.));
#7232=DIRECTION('center_axis',(0.,0.,-1.));
#7233=DIRECTION('ref_axis',(-1.,0.,0.));
#7234=DIRECTION('center_axis',(1.,0.,0.));
#7235=DIRECTION('ref_axis',(0.,-0.70710678118654,-0.707106781186555));
#7236=DIRECTION('',(-1.,0.,0.));
#7237=DIRECTION('',(1.,0.,0.));
#7238=DIRECTION('center_axis',(1.,0.,0.));
#7239=DIRECTION('ref_axis',(0.,0.,-1.));
#7240=DIRECTION('center_axis',(1.,0.,0.));
#7241=DIRECTION('ref_axis',(0.,-1.,0.));
#7242=DIRECTION('center_axis',(0.,0.,-1.));
#7243=DIRECTION('ref_axis',(-1.,0.,0.));
#7244=DIRECTION('center_axis',(0.,1.,0.));
#7245=DIRECTION('ref_axis',(0.,0.,-1.));
#7246=DIRECTION('center_axis',(0.,0.,-1.));
#7247=DIRECTION('ref_axis',(-0.707106781186547,0.707106781186547,0.));
#7248=DIRECTION('',(0.,0.,-1.));
#7249=DIRECTION('center_axis',(-1.,0.,0.));
#7250=DIRECTION('ref_axis',(0.,0.,1.));
#7251=DIRECTION('center_axis',(-1.,0.,0.));
#7252=DIRECTION('ref_axis',(0.,1.,0.));
#7253=DIRECTION('center_axis',(0.,0.,-1.));
#7254=DIRECTION('ref_axis',(1.,0.,0.));
#7255=DIRECTION('center_axis',(0.,-1.,0.));
#7256=DIRECTION('ref_axis',(0.,0.,-1.));
#7257=DIRECTION('center_axis',(0.,0.,1.));
#7258=DIRECTION('ref_axis',(0.707106781186547,-0.707106781186547,0.));
#7259=DIRECTION('',(0.,0.,-1.));
#7260=DIRECTION('center_axis',(0.408248290463863,-0.816496580927726,-0.408248290463863));
#7261=DIRECTION('ref_axis',(0.577350269189626,0.577350269189626,-0.577350269189626));
#7262=DIRECTION('center_axis',(0.,1.,0.));
#7263=DIRECTION('ref_axis',(0.,0.,-1.));
#7264=DIRECTION('center_axis',(1.,0.,0.));
#7265=DIRECTION('ref_axis',(0.,1.,0.));
#7266=DIRECTION('center_axis',(0.,0.,-1.));
#7267=DIRECTION('ref_axis',(1.,0.,0.));
#7268=DIRECTION('center_axis',(1.,0.,0.));
#7269=DIRECTION('ref_axis',(0.,0.,-1.));
#7270=DIRECTION('center_axis',(1.,0.,0.));
#7271=DIRECTION('ref_axis',(0.,0.,1.));
#7272=DIRECTION('center_axis',(0.,-1.,0.));
#7273=DIRECTION('ref_axis',(-1.,0.,0.));
#7274=DIRECTION('center_axis',(0.,0.,-1.));
#7275=DIRECTION('ref_axis',(0.,-1.,0.));
#7276=DIRECTION('center_axis',(-0.408248290463858,-0.816496580927728,-0.408248290463864));
#7277=DIRECTION('ref_axis',(-0.577350269189624,0.577350269189624,-0.57735026918963));
#7278=DIRECTION('center_axis',(0.,0.,-1.));
#7279=DIRECTION('ref_axis',(0.,1.,0.));
#7280=DIRECTION('center_axis',(-1.,0.,0.));
#7281=DIRECTION('ref_axis',(0.,0.,-1.));
#7282=DIRECTION('center_axis',(0.,1.,0.));
#7283=DIRECTION('ref_axis',(-1.,0.,0.));
#7284=DIRECTION('center_axis',(1.,0.,0.));
#7285=DIRECTION('ref_axis',(0.,0.70710678118654,-0.707106781186555));
#7286=DIRECTION('',(-1.,0.,0.));
#7287=DIRECTION('',(1.,0.,0.));
#7288=DIRECTION('center_axis',(0.,-1.,0.));
#7289=DIRECTION('ref_axis',(-0.70710678118655,0.,-0.707106781186545));
#7290=DIRECTION('',(0.,-1.,0.));
#7291=DIRECTION('center_axis',(-0.408248290463858,-0.816496580927728,0.408248290463864));
#7292=DIRECTION('ref_axis',(0.577350269189624,-0.577350269189624,-0.57735026918963));
#7293=DIRECTION('center_axis',(0.,0.,-1.));
#7294=DIRECTION('ref_axis',(0.,-1.,0.));
#7295=DIRECTION('center_axis',(1.,0.,0.));
#7296=DIRECTION('ref_axis',(0.,0.,-1.));
#7297=DIRECTION('center_axis',(0.,-1.,0.));
#7298=DIRECTION('ref_axis',(1.,0.,0.));
#7299=DIRECTION('center_axis',(0.408248290463858,-0.816496580927728,0.408248290463864));
#7300=DIRECTION('ref_axis',(0.577350269189624,0.577350269189624,0.57735026918963));
#7301=DIRECTION('center_axis',(0.,0.,1.));
#7302=DIRECTION('ref_axis',(0.,1.,0.));
#7303=DIRECTION('center_axis',(1.,0.,0.));
#7304=DIRECTION('ref_axis',(0.,0.,1.));
#7305=DIRECTION('center_axis',(0.,1.,0.));
#7306=DIRECTION('ref_axis',(1.,0.,0.));
#7307=DIRECTION('center_axis',(0.408248290463863,-0.816496580927726,0.408248290463863));
#7308=DIRECTION('ref_axis',(-0.577350269189626,-0.577350269189626,-0.577350269189626));
#7309=DIRECTION('center_axis',(0.,-1.,0.));
#7310=DIRECTION('ref_axis',(0.,0.,-1.));
#7311=DIRECTION('center_axis',(-1.,0.,0.));
#7312=DIRECTION('ref_axis',(0.,-1.,0.));
#7313=DIRECTION('center_axis',(0.,0.,-1.));
#7314=DIRECTION('ref_axis',(-1.,0.,0.));
#7315=DIRECTION('center_axis',(1.,0.,0.));
#7316=DIRECTION('ref_axis',(0.,-0.70710678118654,-0.707106781186555));
#7317=DIRECTION('',(-1.,0.,0.));
#7318=DIRECTION('',(1.,0.,0.));
#7319=DIRECTION('center_axis',(-0.408248290463863,-0.816496580927726,0.408248290463863));
#7320=DIRECTION('ref_axis',(-0.577350269189626,0.577350269189626,0.577350269189626));
#7321=DIRECTION('center_axis',(0.,1.,0.));
#7322=DIRECTION('ref_axis',(0.,0.,1.));
#7323=DIRECTION('center_axis',(-1.,0.,0.));
#7324=DIRECTION('ref_axis',(0.,1.,0.));
#7325=DIRECTION('center_axis',(0.,0.,1.));
#7326=DIRECTION('ref_axis',(-1.,0.,0.));
#7327=DIRECTION('center_axis',(1.,0.,0.));
#7328=DIRECTION('ref_axis',(0.,0.707106781186542,0.707106781186553));
#7329=DIRECTION('',(-1.,0.,0.));
#7330=DIRECTION('center_axis',(0.,0.,-1.));
#7331=DIRECTION('ref_axis',(-0.707106781186558,0.707106781186537,0.));
#7332=DIRECTION('',(0.,0.,-1.));
#7333=DIRECTION('center_axis',(-0.408248290463853,-0.81649658092773,-0.408248290463865));
#7334=DIRECTION('ref_axis',(0.577350269189624,-0.577350269189624,0.57735026918963));
#7335=DIRECTION('center_axis',(0.,-1.,0.));
#7336=DIRECTION('ref_axis',(0.,0.,1.));
#7337=DIRECTION('center_axis',(1.,0.,0.));
#7338=DIRECTION('ref_axis',(0.,-1.,0.));
#7339=DIRECTION('center_axis',(0.,-7.40148683083442E-15,1.));
#7340=DIRECTION('ref_axis',(1.,0.,0.));
#7341=DIRECTION('center_axis',(0.408248290463858,-0.816496580927728,-0.408248290463864));
#7342=DIRECTION('ref_axis',(-0.57735026918962,-0.57735026918962,0.577350269189638));
#7343=DIRECTION('center_axis',(7.40148683083442E-15,0.,1.));
#7344=DIRECTION('ref_axis',(0.,-1.,0.));
#7345=DIRECTION('center_axis',(-1.,0.,0.));
#7346=DIRECTION('ref_axis',(0.,0.,1.));
#7347=DIRECTION('center_axis',(0.,-1.,0.));
#7348=DIRECTION('ref_axis',(-1.,0.,0.));
#7349=DIRECTION('center_axis',(1.,0.,0.));
#7350=DIRECTION('ref_axis',(0.,-0.707106781186537,0.707106781186558));
#7351=DIRECTION('',(1.,0.,0.));
#7352=DIRECTION('center_axis',(0.,1.,0.));
#7353=DIRECTION('ref_axis',(-0.707106781186553,0.,0.707106781186542));
#7354=DIRECTION('center_axis',(0.,0.,1.));
#7355=DIRECTION('ref_axis',(-0.707106781186558,-0.707106781186537,0.));
#7356=DIRECTION('',(0.,0.,1.));
#7357=DIRECTION('center_axis',(0.,0.,-1.));
#7358=DIRECTION('ref_axis',(0.707106781186558,-0.707106781186537,0.));
#7359=DIRECTION('',(0.,0.,-1.));
#7360=DIRECTION('center_axis',(0.,-1.,0.));
#7361=DIRECTION('ref_axis',(0.707106781186553,0.,0.707106781186542));
#7362=DIRECTION('center_axis',(0.,-1.,0.));
#7363=DIRECTION('ref_axis',(-0.70710678118655,0.,-0.707106781186545));
#7364=DIRECTION('',(0.,-1.,0.));
#7365=DIRECTION('center_axis',(0.,0.,1.));
#7366=DIRECTION('ref_axis',(0.707106781186558,0.707106781186537,0.));
#7367=DIRECTION('',(0.,0.,1.));
#7368=DIRECTION('center_axis',(0.,1.,0.));
#7369=DIRECTION('ref_axis',(0.70710678118655,0.,-0.707106781186545));
#7370=DIRECTION('',(0.,1.,0.));
#7371=DIRECTION('center_axis',(0.,0.,-1.));
#7372=DIRECTION('ref_axis',(-0.707106781186547,-0.707106781186547,0.));
#7373=DIRECTION('',(0.,0.,1.));
#7374=DIRECTION('center_axis',(1.,0.,0.));
#7375=DIRECTION('ref_axis',(0.,0.70710678118655,0.707106781186545));
#7376=DIRECTION('',(-1.,0.,0.));
#7377=DIRECTION('',(1.,0.,0.));
#7378=DIRECTION('center_axis',(0.,1.,0.));
#7379=DIRECTION('ref_axis',(0.70710678118655,0.,-0.707106781186545));
#7380=DIRECTION('',(0.,1.,0.));
#7381=DIRECTION('center_axis',(-1.,0.,0.));
#7382=DIRECTION('ref_axis',(0.,-0.70710678118655,0.707106781186545));
#7383=DIRECTION('',(1.,0.,0.));
#7384=DIRECTION('',(-1.,0.,0.));
#7385=DIRECTION('center_axis',(0.,1.,0.));
#7386=DIRECTION('ref_axis',(-0.70710678118655,0.,-0.707106781186545));
#7387=DIRECTION('',(0.,-1.,0.));
#7388=DIRECTION('center_axis',(0.,0.,1.));
#7389=DIRECTION('ref_axis',(0.707106781186547,0.707106781186547,0.));
#7390=DIRECTION('',(0.,0.,1.));
#7391=DIRECTION('center_axis',(0.,-1.,0.));
#7392=DIRECTION('ref_axis',(0.70710678118655,0.,-0.707106781186545));
#7393=DIRECTION('',(0.,1.,0.));
#7394=DIRECTION('center_axis',(0.,0.,-1.));
#7395=DIRECTION('ref_axis',(-0.707106781186558,-0.707106781186537,0.));
#7396=DIRECTION('',(0.,0.,1.));
#7397=DIRECTION('center_axis',(1.,0.,0.));
#7398=DIRECTION('ref_axis',(0.,0.70710678118654,0.707106781186555));
#7399=DIRECTION('',(-1.,0.,0.));
#7400=DIRECTION('',(1.,0.,0.));
#7401=DIRECTION('center_axis',(0.,1.,0.));
#7402=DIRECTION('ref_axis',(0.70710678118655,0.,-0.707106781186545));
#7403=DIRECTION('',(0.,1.,0.));
#7404=DIRECTION('center_axis',(0.,0.,1.));
#7405=DIRECTION('ref_axis',(0.707106781186558,-0.707106781186537,0.));
#7406=DIRECTION('',(0.,0.,-1.));
#7407=DIRECTION('center_axis',(-1.,0.,0.));
#7408=DIRECTION('ref_axis',(0.,-0.70710678118654,0.707106781186555));
#7409=DIRECTION('',(1.,0.,0.));
#7410=DIRECTION('',(-1.,0.,0.));
#7411=DIRECTION('center_axis',(0.,0.,1.));
#7412=DIRECTION('ref_axis',(0.707106781186558,0.707106781186537,0.));
#7413=DIRECTION('',(0.,0.,1.));
#7414=DIRECTION('center_axis',(0.,0.,1.));
#7415=DIRECTION('ref_axis',(-0.707106781186553,0.707106781186542,0.));
#7416=DIRECTION('',(0.,0.,-1.));
#7417=DIRECTION('center_axis',(0.,1.,0.));
#7418=DIRECTION('ref_axis',(0.70710678118655,0.,-0.707106781186545));
#7419=DIRECTION('',(0.,1.,0.));
#7420=DIRECTION('center_axis',(0.,0.707106781186548,-0.707106781186548));
#7421=DIRECTION('ref_axis',(0.,-0.707106781186548,-0.707106781186548));
#7422=DIRECTION('center_axis',(0.,0.,-1.));
#7423=DIRECTION('ref_axis',(0.707106781186553,0.707106781186542,0.));
#7424=DIRECTION('',(0.,0.,1.));
#7425=DIRECTION('center_axis',(0.,0.,-1.));
#7426=DIRECTION('ref_axis',(0.707106781186553,-0.707106781186542,0.));
#7427=DIRECTION('',(0.,0.,-1.));
#7428=DIRECTION('center_axis',(0.,0.707106781186548,-0.707106781186548));
#7429=DIRECTION('ref_axis',(0.,0.707106781186547,0.707106781186547));
#7430=DIRECTION('center_axis',(0.,0.,1.));
#7431=DIRECTION('ref_axis',(-0.707106781186553,0.707106781186542,0.));
#7432=DIRECTION('',(0.,0.,-1.));
#7433=DIRECTION('center_axis',(0.,1.,0.));
#7434=DIRECTION('ref_axis',(0.70710678118655,0.,-0.707106781186545));
#7435=DIRECTION('',(0.,1.,0.));
#7436=DIRECTION('center_axis',(0.,0.707106781186548,-0.707106781186548));
#7437=DIRECTION('ref_axis',(0.,-0.707106781186548,-0.707106781186548));
#7438=DIRECTION('center_axis',(0.,0.,-1.));
#7439=DIRECTION('ref_axis',(0.707106781186553,-0.707106781186542,0.));
#7440=DIRECTION('',(0.,0.,-1.));
#7441=DIRECTION('center_axis',(0.,-1.,0.));
#7442=DIRECTION('ref_axis',(0.,0.,-1.));
#7443=DIRECTION('',(1.,0.,0.));
#7444=DIRECTION('',(-1.,0.,0.));
#7445=DIRECTION('center_axis',(0.,0.,-1.));
#7446=DIRECTION('ref_axis',(0.,1.,0.));
#7447=DIRECTION('',(-1.,0.,0.));
#7448=DIRECTION('center_axis',(0.,-1.,0.));
#7449=DIRECTION('ref_axis',(0.,0.,-1.));
#7450=DIRECTION('',(1.,0.,0.));
#7451=DIRECTION('center_axis',(0.,0.,-1.));
#7452=DIRECTION('ref_axis',(0.,1.,0.));
#7453=DIRECTION('',(-1.,0.,0.));
#7454=DIRECTION('center_axis',(0.,-1.,0.));
#7455=DIRECTION('ref_axis',(0.,0.,-1.));
#7456=DIRECTION('',(-1.,0.,0.));
#7457=DIRECTION('center_axis',(0.,0.,1.));
#7458=DIRECTION('ref_axis',(0.,-1.,0.));
#7459=DIRECTION('',(-1.,0.,0.));
#7460=DIRECTION('center_axis',(0.,0.,1.));
#7461=DIRECTION('ref_axis',(0.,-1.,0.));
#7462=DIRECTION('',(-1.,0.,0.));
#7463=DIRECTION('center_axis',(0.,-1.,0.));
#7464=DIRECTION('ref_axis',(0.,0.,-1.));
#7465=DIRECTION('center_axis',(0.,1.,0.));
#7466=DIRECTION('ref_axis',(0.,0.,1.));
#7467=DIRECTION('center_axis',(0.,1.,0.));
#7468=DIRECTION('ref_axis',(0.,0.,1.));
#7469=DIRECTION('center_axis',(0.,0.,-1.));
#7470=DIRECTION('ref_axis',(0.,1.,0.));
#7471=DIRECTION('center_axis',(0.,1.,0.));
#7472=DIRECTION('ref_axis',(0.,0.,1.));
#7473=DIRECTION('center_axis',(0.,0.,1.));
#7474=DIRECTION('ref_axis',(0.,-1.,0.));
#7475=DIRECTION('center_axis',(0.,1.,0.));
#7476=DIRECTION('ref_axis',(0.,0.,1.));
#7477=DIRECTION('center_axis',(0.,0.,-1.));
#7478=DIRECTION('ref_axis',(0.,1.,0.));
#7479=DIRECTION('center_axis',(0.,0.,-1.));
#7480=DIRECTION('ref_axis',(0.,1.,0.));
#7481=DIRECTION('center_axis',(0.,1.,0.));
#7482=DIRECTION('ref_axis',(0.,0.,1.));
#7483=DIRECTION('center_axis',(0.,-1.,0.));
#7484=DIRECTION('ref_axis',(0.,0.,-1.));
#7485=DIRECTION('center_axis',(0.,0.,-1.));
#7486=DIRECTION('ref_axis',(0.,1.,0.));
#7487=DIRECTION('center_axis',(0.,0.,1.));
#7488=DIRECTION('ref_axis',(-1.,0.,0.));
#7489=DIRECTION('center_axis',(0.,0.,1.));
#7490=DIRECTION('ref_axis',(-1.,0.,0.));
#7491=DIRECTION('center_axis',(0.,0.,1.));
#7492=DIRECTION('ref_axis',(-1.,0.,0.));
#7493=DIRECTION('center_axis',(0.,0.,1.));
#7494=DIRECTION('ref_axis',(-1.,0.,0.));
#7495=DIRECTION('center_axis',(0.,0.,1.));
#7496=DIRECTION('ref_axis',(-1.,0.,0.));
#7497=DIRECTION('center_axis',(0.,0.,1.));
#7498=DIRECTION('ref_axis',(-1.,0.,0.));
#7499=DIRECTION('center_axis',(0.,0.,1.));
#7500=DIRECTION('ref_axis',(-1.,0.,0.));
#7501=DIRECTION('center_axis',(0.,0.,1.));
#7502=DIRECTION('ref_axis',(-1.,0.,0.));
#7503=DIRECTION('center_axis',(0.,0.,1.));
#7504=DIRECTION('ref_axis',(-1.,0.,0.));
#7505=DIRECTION('center_axis',(0.,0.,1.));
#7506=DIRECTION('ref_axis',(-1.,0.,0.));
#7507=DIRECTION('center_axis',(0.,0.,1.));
#7508=DIRECTION('ref_axis',(-1.,0.,0.));
#7509=DIRECTION('center_axis',(0.,0.,1.));
#7510=DIRECTION('ref_axis',(-1.,0.,0.));
#7511=DIRECTION('center_axis',(0.,0.,1.));
#7512=DIRECTION('ref_axis',(-1.,0.,0.));
#7513=DIRECTION('center_axis',(0.,0.,1.));
#7514=DIRECTION('ref_axis',(-1.,0.,0.));
#7515=DIRECTION('center_axis',(0.,0.,1.));
#7516=DIRECTION('ref_axis',(-1.,0.,0.));
#7517=DIRECTION('center_axis',(0.,0.,1.));
#7518=DIRECTION('ref_axis',(-1.,0.,0.));
#7519=DIRECTION('axis',(0.,0.,1.));
#7520=DIRECTION('refdir',(1.,0.,0.));
#7521=DIRECTION('center_axis',(-1.,0.,0.));
#7522=DIRECTION('ref_axis',(0.,0.,1.));
#7523=DIRECTION('center_axis',(-1.,0.,0.));
#7524=DIRECTION('ref_axis',(0.,1.,0.));
#7525=DIRECTION('center_axis',(0.,-1.,0.));
#7526=DIRECTION('ref_axis',(0.,0.,-1.));
#7527=DIRECTION('center_axis',(1.,0.,0.));
#7528=DIRECTION('ref_axis',(0.,1.,0.));
#7529=DIRECTION('center_axis',(1.,0.,0.));
#7530=DIRECTION('ref_axis',(0.,1.,0.));
#7531=DIRECTION('center_axis',(1.,0.,0.));
#7532=DIRECTION('ref_axis',(0.,1.,0.));
#7533=DIRECTION('center_axis',(1.,0.,0.));
#7534=DIRECTION('ref_axis',(0.,1.,0.));
#7535=DIRECTION('center_axis',(-1.,0.,0.));
#7536=DIRECTION('ref_axis',(0.,1.,0.));
#7537=DIRECTION('',(-1.,0.,0.));
#7538=DIRECTION('center_axis',(-1.,0.,0.));
#7539=DIRECTION('ref_axis',(0.,1.,0.));
#7540=DIRECTION('center_axis',(-1.,0.,0.));
#7541=DIRECTION('ref_axis',(0.,1.,0.));
#7542=DIRECTION('center_axis',(1.,0.,0.));
#7543=DIRECTION('ref_axis',(0.,0.,-1.));
#7544=DIRECTION('center_axis',(0.,-1.,0.));
#7545=DIRECTION('ref_axis',(0.,0.,1.));
#7546=DIRECTION('center_axis',(-1.,0.,0.));
#7547=DIRECTION('ref_axis',(0.,1.,0.));
#7548=DIRECTION('center_axis',(-1.,0.,0.));
#7549=DIRECTION('ref_axis',(0.,1.,0.));
#7550=DIRECTION('center_axis',(-1.,0.,0.));
#7551=DIRECTION('ref_axis',(0.,1.,0.));
#7552=DIRECTION('',(-1.,0.,0.));
#7553=DIRECTION('center_axis',(1.,0.,0.));
#7554=DIRECTION('ref_axis',(0.,1.,0.));
#7555=DIRECTION('center_axis',(1.,0.,0.));
#7556=DIRECTION('ref_axis',(0.,1.,0.));
#7557=DIRECTION('center_axis',(1.,0.,0.));
#7558=DIRECTION('ref_axis',(0.,0.,-1.));
#7559=DIRECTION('center_axis',(1.,0.,0.));
#7560=DIRECTION('ref_axis',(0.,1.,0.));
#7561=DIRECTION('center_axis',(0.,-1.,0.));
#7562=DIRECTION('ref_axis',(0.,0.,1.));
#7563=DIRECTION('center_axis',(1.,0.,0.));
#7564=DIRECTION('ref_axis',(0.,1.,0.));
#7565=DIRECTION('center_axis',(-1.,0.,0.));
#7566=DIRECTION('ref_axis',(0.,1.,0.));
#7567=DIRECTION('center_axis',(-1.,0.,0.));
#7568=DIRECTION('ref_axis',(0.,0.,1.));
#7569=DIRECTION('center_axis',(0.,-1.,0.));
#7570=DIRECTION('ref_axis',(0.,0.,-1.));
#7571=DIRECTION('axis',(0.,0.,1.));
#7572=DIRECTION('refdir',(1.,0.,0.));
#7573=DIRECTION('center_axis',(1.,0.,0.));
#7574=DIRECTION('ref_axis',(0.,0.,1.));
#7575=DIRECTION('center_axis',(-1.,0.,0.));
#7576=DIRECTION('ref_axis',(0.,1.,0.));
#7577=DIRECTION('center_axis',(0.,1.,0.));
#7578=DIRECTION('ref_axis',(0.,0.,-1.));
#7579=DIRECTION('center_axis',(1.,0.,0.));
#7580=DIRECTION('ref_axis',(0.,1.,0.));
#7581=DIRECTION('center_axis',(1.,0.,0.));
#7582=DIRECTION('ref_axis',(0.,1.,0.));
#7583=DIRECTION('center_axis',(1.,0.,0.));
#7584=DIRECTION('ref_axis',(0.,1.,0.));
#7585=DIRECTION('center_axis',(1.,0.,0.));
#7586=DIRECTION('ref_axis',(0.,1.,0.));
#7587=DIRECTION('center_axis',(-1.,0.,0.));
#7588=DIRECTION('ref_axis',(0.,1.,0.));
#7589=DIRECTION('',(1.,0.,0.));
#7590=DIRECTION('center_axis',(-1.,0.,0.));
#7591=DIRECTION('ref_axis',(0.,1.,0.));
#7592=DIRECTION('center_axis',(-1.,0.,0.));
#7593=DIRECTION('ref_axis',(0.,1.,0.));
#7594=DIRECTION('center_axis',(-1.,0.,0.));
#7595=DIRECTION('ref_axis',(0.,0.,-1.));
#7596=DIRECTION('center_axis',(0.,1.,0.));
#7597=DIRECTION('ref_axis',(0.,0.,1.));
#7598=DIRECTION('center_axis',(-1.,0.,0.));
#7599=DIRECTION('ref_axis',(0.,1.,0.));
#7600=DIRECTION('center_axis',(-1.,0.,0.));
#7601=DIRECTION('ref_axis',(0.,1.,0.));
#7602=DIRECTION('center_axis',(-1.,0.,0.));
#7603=DIRECTION('ref_axis',(0.,1.,0.));
#7604=DIRECTION('',(1.,0.,0.));
#7605=DIRECTION('center_axis',(1.,0.,0.));
#7606=DIRECTION('ref_axis',(0.,1.,0.));
#7607=DIRECTION('center_axis',(1.,0.,0.));
#7608=DIRECTION('ref_axis',(0.,1.,0.));
#7609=DIRECTION('center_axis',(-1.,0.,0.));
#7610=DIRECTION('ref_axis',(0.,0.,-1.));
#7611=DIRECTION('center_axis',(1.,0.,0.));
#7612=DIRECTION('ref_axis',(0.,1.,0.));
#7613=DIRECTION('center_axis',(0.,1.,0.));
#7614=DIRECTION('ref_axis',(0.,0.,1.));
#7615=DIRECTION('center_axis',(1.,0.,0.));
#7616=DIRECTION('ref_axis',(0.,1.,0.));
#7617=DIRECTION('center_axis',(-1.,0.,0.));
#7618=DIRECTION('ref_axis',(0.,1.,0.));
#7619=DIRECTION('center_axis',(1.,0.,0.));
#7620=DIRECTION('ref_axis',(0.,0.,1.));
#7621=DIRECTION('center_axis',(0.,1.,0.));
#7622=DIRECTION('ref_axis',(0.,0.,-1.));
#7623=DIRECTION('axis',(0.,0.,1.));
#7624=DIRECTION('refdir',(1.,0.,0.));
#7625=DIRECTION('center_axis',(0.,0.,1.));
#7626=DIRECTION('ref_axis',(-1.,0.,0.));
#7627=DIRECTION('center_axis',(0.,0.,1.));
#7628=DIRECTION('ref_axis',(-1.,0.,0.));
#7629=DIRECTION('center_axis',(0.,1.,0.));
#7630=DIRECTION('ref_axis',(1.,0.,0.));
#7631=DIRECTION('center_axis',(0.,0.,-1.));
#7632=DIRECTION('ref_axis',(-1.,0.,0.));
#7633=DIRECTION('center_axis',(0.,0.,-1.));
#7634=DIRECTION('ref_axis',(-1.,0.,0.));
#7635=DIRECTION('',(-1.,0.,0.));
#7636=DIRECTION('',(0.,-1.,0.));
#7637=DIRECTION('',(1.,-2.77555756156289E-16,0.));
#7638=DIRECTION('',(5.9211894646675E-16,1.,0.));
#7639=DIRECTION('center_axis',(0.,0.,-1.));
#7640=DIRECTION('ref_axis',(-1.,0.,0.));
#7641=DIRECTION('center_axis',(0.,0.,1.));
#7642=DIRECTION('ref_axis',(-1.,0.,0.));
#7643=DIRECTION('',(0.,0.,-1.));
#7644=DIRECTION('center_axis',(0.,0.,1.));
#7645=DIRECTION('ref_axis',(-1.,0.,0.));
#7646=DIRECTION('center_axis',(0.,0.,1.));
#7647=DIRECTION('ref_axis',(-1.,0.,0.));
#7648=DIRECTION('center_axis',(0.,0.,1.));
#7649=DIRECTION('ref_axis',(-1.,0.,0.));
#7650=DIRECTION('center_axis',(0.,1.,0.));
#7651=DIRECTION('ref_axis',(1.,0.,0.));
#7652=DIRECTION('center_axis',(0.,0.,1.));
#7653=DIRECTION('ref_axis',(-1.,0.,0.));
#7654=DIRECTION('',(0.,0.,-1.));
#7655=DIRECTION('center_axis',(0.,0.,1.));
#7656=DIRECTION('ref_axis',(-1.,0.,0.));
#7657=DIRECTION('center_axis',(0.,0.,-1.));
#7658=DIRECTION('ref_axis',(1.,0.,0.));
#7659=DIRECTION('center_axis',(0.,0.,-1.));
#7660=DIRECTION('ref_axis',(-1.,0.,0.));
#7661=DIRECTION('center_axis',(0.,1.,0.));
#7662=DIRECTION('ref_axis',(-1.,0.,0.));
#7663=DIRECTION('center_axis',(0.,0.,1.));
#7664=DIRECTION('ref_axis',(-1.,0.,0.));
#7665=DIRECTION('center_axis',(0.,0.,1.));
#7666=DIRECTION('ref_axis',(-1.,0.,0.));
#7667=DIRECTION('center_axis',(0.,0.,1.));
#7668=DIRECTION('ref_axis',(-1.,0.,0.));
#7669=DIRECTION('',(-1.,0.,0.));
#7670=DIRECTION('',(0.,-1.,0.));
#7671=DIRECTION('',(1.,0.,0.));
#7672=DIRECTION('',(5.9211894646675E-16,1.,0.));
#7673=DIRECTION('center_axis',(0.,0.,-1.));
#7674=DIRECTION('ref_axis',(-1.,0.,0.));
#7675=DIRECTION('center_axis',(0.,0.,-1.));
#7676=DIRECTION('ref_axis',(-1.,0.,0.));
#7677=DIRECTION('',(0.,0.,-1.));
#7678=DIRECTION('center_axis',(0.,0.,-1.));
#7679=DIRECTION('ref_axis',(-1.,0.,0.));
#7680=DIRECTION('center_axis',(0.,0.,-1.));
#7681=DIRECTION('ref_axis',(1.,0.,0.));
#7682=DIRECTION('center_axis',(0.,1.,0.));
#7683=DIRECTION('ref_axis',(-1.,0.,0.));
#7684=DIRECTION('center_axis',(0.,0.,1.));
#7685=DIRECTION('ref_axis',(-1.,0.,0.));
#7686=DIRECTION('center_axis',(0.,0.,1.));
#7687=DIRECTION('ref_axis',(-1.,0.,0.));
#7688=DIRECTION('center_axis',(0.,0.,-1.));
#7689=DIRECTION('ref_axis',(-1.,0.,0.));
#7690=DIRECTION('',(0.,0.,-1.));
#7691=DIRECTION('center_axis',(0.,0.,-1.));
#7692=DIRECTION('ref_axis',(-1.,0.,0.));
#7693=DIRECTION('center_axis',(-0.408248290463861,0.408248290463837,-0.81649658092774));
#7694=DIRECTION('ref_axis',(0.577350269189669,-0.577350269189598,-0.57735026918961));
#7695=DIRECTION('center_axis',(0.,7.40148683083442E-15,1.));
#7696=DIRECTION('ref_axis',(1.,0.,0.));
#7697=DIRECTION('center_axis',(-1.,0.,5.92118946466745E-14));
#7698=DIRECTION('ref_axis',(0.,-1.,0.));
#7699=DIRECTION('center_axis',(0.,1.,0.));
#7700=DIRECTION('ref_axis',(0.,0.,-1.));
#7701=DIRECTION('center_axis',(0.408248290463865,-0.81649658092773,0.408248290463853));
#7702=DIRECTION('ref_axis',(-0.577350269189602,-0.577350269189626,-0.577350269189649));
#7703=DIRECTION('center_axis',(1.,0.,0.));
#7704=DIRECTION('ref_axis',(0.,0.,-1.));
#7705=DIRECTION('center_axis',(-7.40148683083454E-15,0.,1.));
#7706=DIRECTION('ref_axis',(0.,-1.,0.));
#7707=DIRECTION('center_axis',(0.,1.,2.96059473233375E-14));
#7708=DIRECTION('ref_axis',(-1.,0.,0.));
#7709=DIRECTION('center_axis',(0.816496580927716,-0.408248290463882,0.408248290463864));
#7710=DIRECTION('ref_axis',(0.577350269189634,0.577350269189634,-0.57735026918961));
#7711=DIRECTION('center_axis',(-1.,0.,0.));
#7712=DIRECTION('ref_axis',(0.,0.,-1.));
#7713=DIRECTION('center_axis',(0.,0.,1.));
#7714=DIRECTION('ref_axis',(0.,1.,0.));
#7715=DIRECTION('center_axis',(0.,-1.,0.));
#7716=DIRECTION('ref_axis',(1.,0.,0.));
#7717=DIRECTION('center_axis',(-5.9211894646675E-16,-1.,0.));
#7718=DIRECTION('ref_axis',(0.707106781186563,0.,-0.707106781186532));
#7719=DIRECTION('',(5.9211894646675E-16,1.,0.));
#7720=DIRECTION('',(-5.9211894646675E-16,-1.,0.));
#7721=DIRECTION('center_axis',(0.816496580927728,0.408248290463864,-0.408248290463858));
#7722=DIRECTION('ref_axis',(0.577350269189594,-0.577350269189642,0.577350269189642));
#7723=DIRECTION('center_axis',(0.,1.,0.));
#7724=DIRECTION('ref_axis',(1.,0.,0.));
#7725=DIRECTION('center_axis',(-1.,0.,0.));
#7726=DIRECTION('ref_axis',(0.,0.,1.));
#7727=DIRECTION('center_axis',(-7.40148683083454E-15,0.,-1.));
#7728=DIRECTION('ref_axis',(0.,-1.,0.));
#7729=DIRECTION('center_axis',(0.,0.,-1.));
#7730=DIRECTION('ref_axis',(0.707106781186516,-0.707106781186579,0.));
#7731=DIRECTION('',(0.,0.,1.));
#7732=DIRECTION('',(0.,0.,-1.));
#7733=DIRECTION('center_axis',(-0.408248290463855,-0.816496580927734,-0.408248290463855));
#7734=DIRECTION('ref_axis',(-0.577350269189651,0.577350269189604,-0.577350269189622));
#7735=DIRECTION('center_axis',(0.,0.,1.));
#7736=DIRECTION('ref_axis',(-1.,0.,0.));
#7737=DIRECTION('center_axis',(1.,0.,0.));
#7738=DIRECTION('ref_axis',(0.,1.,0.));
#7739=DIRECTION('center_axis',(0.,-1.,0.));
#7740=DIRECTION('ref_axis',(0.,0.,-1.));
#7741=DIRECTION('center_axis',(0.,-1.,0.));
#7742=DIRECTION('ref_axis',(-0.707106781186563,0.,-0.707106781186532));
#7743=DIRECTION('',(0.,1.,0.));
#7744=DIRECTION('',(0.,-1.,0.));
#7745=DIRECTION('center_axis',(-1.,0.,0.));
#7746=DIRECTION('ref_axis',(0.,0.707106781186553,-0.707106781186542));
#7747=DIRECTION('',(1.,0.,0.));
#7748=DIRECTION('',(-1.,0.,0.));
#7749=DIRECTION('center_axis',(0.408248290463864,-0.816496580927728,-0.408248290463858));
#7750=DIRECTION('ref_axis',(-0.5773502691896,-0.577350269189624,0.577350269189653));
#7751=DIRECTION('center_axis',(1.,0.,0.));
#7752=DIRECTION('ref_axis',(0.,-1.,0.));
#7753=DIRECTION('center_axis',(-1.48029736616691E-14,1.,0.));
#7754=DIRECTION('ref_axis',(0.,0.,1.));
#7755=DIRECTION('center_axis',(0.,-7.40148683083454E-15,-1.));
#7756=DIRECTION('ref_axis',(-1.,0.,0.));
#7757=DIRECTION('center_axis',(0.,0.,-1.));
#7758=DIRECTION('ref_axis',(-0.707106781186568,-0.707106781186527,0.));
#7759=DIRECTION('',(0.,0.,1.));
#7760=DIRECTION('',(0.,0.,-1.));
#7761=DIRECTION('center_axis',(0.408248290463856,-0.816496580927712,0.408248290463898));
#7762=DIRECTION('ref_axis',(0.577350269189574,0.577350269189645,0.577350269189657));
#7763=DIRECTION('center_axis',(0.,0.,-1.));
#7764=DIRECTION('ref_axis',(1.,0.,0.));
#7765=DIRECTION('center_axis',(-1.,0.,5.9211894646675E-14));
#7766=DIRECTION('ref_axis',(0.,1.,0.));
#7767=DIRECTION('center_axis',(-1.48029736616699E-14,-1.,0.));
#7768=DIRECTION('ref_axis',(0.,0.,1.));
#7769=DIRECTION('center_axis',(-1.,0.,0.));
#7770=DIRECTION('ref_axis',(0.,0.,-1.));
#7771=DIRECTION('center_axis',(1.,0.,0.));
#7772=DIRECTION('ref_axis',(0.,1.,0.));
#7773=DIRECTION('center_axis',(0.,1.,0.));
#7774=DIRECTION('ref_axis',(0.,0.,1.));
#7775=DIRECTION('center_axis',(-1.,5.9211894646675E-16,0.));
#7776=DIRECTION('ref_axis',(0.,0.707106781186545,-0.70710678118655));
#7777=DIRECTION('center_axis',(0.,0.,-1.));
#7778=DIRECTION('ref_axis',(1.,0.,0.));
#7779=DIRECTION('center_axis',(-0.408248290463862,-0.816496580927724,0.408248290463868));
#7780=DIRECTION('ref_axis',(-0.57735026918959,0.577350269189638,0.577350269189649));
#7781=DIRECTION('center_axis',(0.,0.,-1.));
#7782=DIRECTION('ref_axis',(0.,1.,0.));
#7783=DIRECTION('center_axis',(0.,-1.,0.));
#7784=DIRECTION('ref_axis',(-1.,0.,0.));
#7785=DIRECTION('center_axis',(1.,0.,0.));
#7786=DIRECTION('ref_axis',(0.,0.,1.));
#7787=DIRECTION('center_axis',(1.,0.,0.));
#7788=DIRECTION('ref_axis',(0.,0.707106781186542,0.707106781186553));
#7789=DIRECTION('',(1.,0.,0.));
#7790=DIRECTION('center_axis',(-1.,0.,0.));
#7791=DIRECTION('ref_axis',(0.,0.,-1.));
#7792=DIRECTION('center_axis',(1.,0.,0.));
#7793=DIRECTION('ref_axis',(0.,0.707106781186545,-0.70710678118655));
#7794=DIRECTION('center_axis',(0.,1.,0.));
#7795=DIRECTION('ref_axis',(-1.,0.,0.));
#7796=DIRECTION('center_axis',(-1.,0.,0.));
#7797=DIRECTION('ref_axis',(0.,0.,-1.));
#7798=DIRECTION('center_axis',(0.,0.,-1.));
#7799=DIRECTION('ref_axis',(0.,-1.,0.));
#7800=DIRECTION('center_axis',(1.,0.,0.));
#7801=DIRECTION('ref_axis',(0.,0.,1.));
#7802=DIRECTION('center_axis',(-1.,5.9211894646675E-16,0.));
#7803=DIRECTION('ref_axis',(0.,-0.70710678118654,-0.707106781186555));
#7804=DIRECTION('center_axis',(0.,-1.,0.));
#7805=DIRECTION('ref_axis',(1.,0.,0.));
#7806=DIRECTION('center_axis',(1.,-5.92118946466763E-14,0.));
#7807=DIRECTION('ref_axis',(0.,0.,-1.));
#7808=DIRECTION('center_axis',(0.,0.,-1.));
#7809=DIRECTION('ref_axis',(0.,1.,0.));
#7810=DIRECTION('center_axis',(-0.408248290463862,-0.816496580927724,-0.408248290463868));
#7811=DIRECTION('ref_axis',(0.577350269189592,-0.577350269189639,0.577350269189645));
#7812=DIRECTION('center_axis',(0.,1.,0.));
#7813=DIRECTION('ref_axis',(1.,0.,0.));
#7814=DIRECTION('center_axis',(-1.,-5.92118946466754E-14,0.));
#7815=DIRECTION('ref_axis',(0.,0.,1.));
#7816=DIRECTION('center_axis',(0.,0.,-1.));
#7817=DIRECTION('ref_axis',(0.,-1.,0.));
#7818=DIRECTION('center_axis',(0.,0.,1.));
#7819=DIRECTION('ref_axis',(0.707106781186527,-0.707106781186568,0.));
#7820=DIRECTION('',(0.,0.,-1.));
#7821=DIRECTION('',(0.,0.,1.));
#7822=DIRECTION('center_axis',(1.,0.,0.));
#7823=DIRECTION('ref_axis',(0.,0.,1.));
#7824=DIRECTION('center_axis',(-1.,0.,0.));
#7825=DIRECTION('ref_axis',(0.,-1.,0.));
#7826=DIRECTION('center_axis',(0.,-1.,0.));
#7827=DIRECTION('ref_axis',(0.,0.,1.));
#7828=DIRECTION('center_axis',(1.,0.,0.));
#7829=DIRECTION('ref_axis',(0.,-0.70710678118654,-0.707106781186555));
#7830=DIRECTION('center_axis',(0.,0.,-1.));
#7831=DIRECTION('ref_axis',(-1.,0.,0.));
#7832=DIRECTION('center_axis',(0.408248290463867,-0.816496580927722,-0.408248290463867));
#7833=DIRECTION('ref_axis',(-0.5773502691896,-0.577350269189636,0.577350269189642));
#7834=DIRECTION('center_axis',(1.,0.,0.));
#7835=DIRECTION('ref_axis',(0.,-1.,0.));
#7836=DIRECTION('center_axis',(0.,1.,0.));
#7837=DIRECTION('ref_axis',(0.,0.,1.));
#7838=DIRECTION('center_axis',(0.,0.,-1.));
#7839=DIRECTION('ref_axis',(-1.,0.,0.));
#7840=DIRECTION('center_axis',(0.,0.,-1.));
#7841=DIRECTION('ref_axis',(-0.707106781186568,-0.707106781186527,0.));
#7842=DIRECTION('',(0.,0.,1.));
#7843=DIRECTION('',(0.,0.,-1.));
#7844=DIRECTION('center_axis',(0.408248290463866,-0.81649658092772,0.408248290463872));
#7845=DIRECTION('ref_axis',(0.577350269189592,0.577350269189628,0.577350269189657));
#7846=DIRECTION('center_axis',(-1.,0.,-5.9211894646675E-14));
#7847=DIRECTION('ref_axis',(0.,1.,0.));
#7848=DIRECTION('center_axis',(1.48029736616682E-14,-1.,0.));
#7849=DIRECTION('ref_axis',(0.,0.,1.));
#7850=DIRECTION('center_axis',(0.,0.,-1.));
#7851=DIRECTION('ref_axis',(1.,0.,0.));
#7852=DIRECTION('center_axis',(0.,0.,-1.));
#7853=DIRECTION('ref_axis',(0.707106781186527,0.707106781186568,0.));
#7854=DIRECTION('',(0.,0.,1.));
#7855=DIRECTION('',(0.,0.,-1.));
#7856=DIRECTION('center_axis',(0.408248290463859,0.408248290463847,-0.816496580927736));
#7857=DIRECTION('ref_axis',(0.577350269189657,0.577350269189622,0.577350269189598));
#7858=DIRECTION('center_axis',(0.,-7.40148683083442E-15,-1.));
#7859=DIRECTION('ref_axis',(1.,0.,0.));
#7860=DIRECTION('center_axis',(-1.,0.,0.));
#7861=DIRECTION('ref_axis',(0.,1.,0.));
#7862=DIRECTION('center_axis',(0.,-1.,0.));
#7863=DIRECTION('ref_axis',(0.,0.,1.));
#7864=DIRECTION('center_axis',(5.9211894646675E-16,1.,0.));
#7865=DIRECTION('ref_axis',(0.707106781186563,0.,0.707106781186532));
#7866=DIRECTION('',(-5.9211894646675E-16,-1.,0.));
#7867=DIRECTION('',(5.9211894646675E-16,1.,0.));
#7868=DIRECTION('center_axis',(-0.408248290463865,-0.81649658092773,0.408248290463853));
#7869=DIRECTION('ref_axis',(-0.5773502691896,0.577350269189624,0.577350269189653));
#7870=DIRECTION('center_axis',(0.,-1.,-2.96059473233375E-14));
#7871=DIRECTION('ref_axis',(-1.,0.,0.));
#7872=DIRECTION('center_axis',(1.,0.,0.));
#7873=DIRECTION('ref_axis',(0.,0.,1.));
#7874=DIRECTION('center_axis',(0.,0.,-1.));
#7875=DIRECTION('ref_axis',(0.,1.,0.));
#7876=DIRECTION('center_axis',(0.,0.,-1.));
#7877=DIRECTION('ref_axis',(-0.707106781186568,0.707106781186527,0.));
#7878=DIRECTION('',(0.,0.,1.));
#7879=DIRECTION('',(0.,0.,-1.));
#7880=DIRECTION('center_axis',(-1.,2.77555756156289E-16,0.));
#7881=DIRECTION('ref_axis',(0.,0.707106781186553,0.707106781186542));
#7882=DIRECTION('',(1.,-2.77555756156289E-16,0.));
#7883=DIRECTION('',(-1.,2.77555756156289E-16,0.));
#7884=DIRECTION('center_axis',(-0.408248290463862,-0.816496580927724,0.408248290463868));
#7885=DIRECTION('ref_axis',(-0.57735026918959,0.577350269189638,0.577350269189649));
#7886=DIRECTION('center_axis',(0.,-1.,0.));
#7887=DIRECTION('ref_axis',(-1.,0.,0.));
#7888=DIRECTION('center_axis',(1.,0.,0.));
#7889=DIRECTION('ref_axis',(0.,0.,1.));
#7890=DIRECTION('center_axis',(-7.40148683083454E-15,0.,-1.));
#7891=DIRECTION('ref_axis',(0.,1.,0.));
#7892=DIRECTION('center_axis',(0.408248290463859,-0.408248290463835,-0.816496580927742));
#7893=DIRECTION('ref_axis',(0.577350269189663,-0.577350269189604,0.57735026918961));
#7894=DIRECTION('center_axis',(7.40148683083454E-15,0.,-1.));
#7895=DIRECTION('ref_axis',(0.,-1.,0.));
#7896=DIRECTION('center_axis',(0.,1.,0.));
#7897=DIRECTION('ref_axis',(1.,0.,0.));
#7898=DIRECTION('center_axis',(-1.,-5.92118946466754E-14,0.));
#7899=DIRECTION('ref_axis',(0.,0.,1.));
#7900=DIRECTION('center_axis',(0.,0.,1.));
#7901=DIRECTION('ref_axis',(0.707106781186516,0.707106781186579,0.));
#7902=DIRECTION('',(0.,0.,1.));
#7903=DIRECTION('',(0.,0.,-1.));
#7904=DIRECTION('center_axis',(0.816496580927732,-0.408248290463866,0.408248290463848));
#7905=DIRECTION('ref_axis',(-0.577350269189588,-0.577350269189659,0.57735026918963));
#7906=DIRECTION('center_axis',(0.,7.40148683083454E-15,-1.));
#7907=DIRECTION('ref_axis',(-1.,0.,0.));
#7908=DIRECTION('center_axis',(1.,0.,0.));
#7909=DIRECTION('ref_axis',(0.,-1.,0.));
#7910=DIRECTION('center_axis',(-2.96059473233381E-14,1.,0.));
#7911=DIRECTION('ref_axis',(0.,0.,1.));
#7912=DIRECTION('center_axis',(0.,-1.,0.));
#7913=DIRECTION('ref_axis',(-0.707106781186563,0.,0.707106781186532));
#7914=DIRECTION('',(0.,1.,0.));
#7915=DIRECTION('',(0.,-1.,0.));
#7916=DIRECTION('center_axis',(1.,0.,0.));
#7917=DIRECTION('ref_axis',(0.,-0.707106781186547,0.707106781186547));
#7918=DIRECTION('',(-1.,0.,0.));
#7919=DIRECTION('',(1.,0.,0.));
#7920=DIRECTION('center_axis',(0.,0.,-1.));
#7921=DIRECTION('ref_axis',(-0.707106781186558,0.707106781186537,0.));
#7922=DIRECTION('',(0.,0.,1.));
#7923=DIRECTION('',(0.,0.,-1.));
#7924=DIRECTION('center_axis',(0.,0.,-1.));
#7925=DIRECTION('ref_axis',(0.707106781186516,-0.707106781186579,0.));
#7926=DIRECTION('',(0.,0.,1.));
#7927=DIRECTION('',(0.,0.,-1.));
#7928=DIRECTION('center_axis',(0.,0.,1.));
#7929=DIRECTION('ref_axis',(-0.707106781186568,-0.707106781186527,0.));
#7930=DIRECTION('',(0.,0.,1.));
#7931=DIRECTION('',(0.,0.,-1.));
#7932=DIRECTION('center_axis',(0.816496580927728,0.408248290463864,-0.408248290463858));
#7933=DIRECTION('ref_axis',(0.577350269189588,-0.577350269189647,0.577350269189642));
#7934=DIRECTION('center_axis',(0.,0.,-1.));
#7935=DIRECTION('ref_axis',(0.,-1.,0.));
#7936=DIRECTION('center_axis',(0.,1.,0.));
#7937=DIRECTION('ref_axis',(1.,0.,0.));
#7938=DIRECTION('center_axis',(-1.,0.,0.));
#7939=DIRECTION('ref_axis',(0.,0.,1.));
#7940=DIRECTION('center_axis',(0.408248290463857,-0.816496580927726,-0.408248290463869));
#7941=DIRECTION('ref_axis',(-0.57735026918959,-0.577350269189638,0.577350269189649));
#7942=DIRECTION('center_axis',(0.,0.,-1.));
#7943=DIRECTION('ref_axis',(-1.,0.,0.));
#7944=DIRECTION('center_axis',(1.,0.,0.));
#7945=DIRECTION('ref_axis',(0.,-1.,0.));
#7946=DIRECTION('center_axis',(0.,1.,0.));
#7947=DIRECTION('ref_axis',(0.,0.,1.));
#7948=DIRECTION('center_axis',(0.408248290463861,0.408248290463837,-0.81649658092774));
#7949=DIRECTION('ref_axis',(0.577350269189665,0.577350269189606,0.577350269189606));
#7950=DIRECTION('center_axis',(0.,0.,-1.));
#7951=DIRECTION('ref_axis',(1.,0.,0.));
#7952=DIRECTION('center_axis',(-1.,0.,-5.9211894646675E-14));
#7953=DIRECTION('ref_axis',(0.,1.,0.));
#7954=DIRECTION('center_axis',(0.,-1.,0.));
#7955=DIRECTION('ref_axis',(0.,0.,1.));
#7956=DIRECTION('center_axis',(5.9211894646675E-16,1.,0.));
#7957=DIRECTION('ref_axis',(0.707106781186563,0.,0.707106781186532));
#7958=DIRECTION('',(-5.9211894646675E-16,-1.,0.));
#7959=DIRECTION('',(5.9211894646675E-16,1.,0.));
#7960=DIRECTION('center_axis',(-0.408248290463868,-0.816496580927724,0.408248290463862));
#7961=DIRECTION('ref_axis',(-0.577350269189598,0.577350269189634,0.577350269189645));
#7962=DIRECTION('center_axis',(0.,-1.,0.));
#7963=DIRECTION('ref_axis',(-1.,0.,0.));
#7964=DIRECTION('center_axis',(1.,0.,0.));
#7965=DIRECTION('ref_axis',(0.,0.,1.));
#7966=DIRECTION('center_axis',(0.,0.,-1.));
#7967=DIRECTION('ref_axis',(0.,1.,0.));
#7968=DIRECTION('center_axis',(0.,0.,-1.));
#7969=DIRECTION('ref_axis',(-0.707106781186568,0.707106781186527,0.));
#7970=DIRECTION('',(0.,0.,1.));
#7971=DIRECTION('',(0.,0.,-1.));
#7972=DIRECTION('center_axis',(-1.,0.,0.));
#7973=DIRECTION('ref_axis',(0.,0.707106781186553,0.707106781186542));
#7974=DIRECTION('',(1.,0.,0.));
#7975=DIRECTION('',(-1.,0.,0.));
#7976=DIRECTION('center_axis',(0.,-1.,0.));
#7977=DIRECTION('ref_axis',(-0.707106781186563,0.,0.707106781186532));
#7978=DIRECTION('',(0.,1.,0.));
#7979=DIRECTION('',(0.,-1.,0.));
#7980=DIRECTION('center_axis',(0.,0.,1.));
#7981=DIRECTION('ref_axis',(0.707106781186516,0.707106781186579,0.));
#7982=DIRECTION('',(0.,0.,1.));
#7983=DIRECTION('',(0.,0.,-1.));
#7984=DIRECTION('center_axis',(1.,0.,0.));
#7985=DIRECTION('ref_axis',(0.,-0.707106781186553,0.707106781186542));
#7986=DIRECTION('',(-1.,0.,0.));
#7987=DIRECTION('',(1.,0.,0.));
#7988=DIRECTION('center_axis',(0.,0.,1.));
#7989=DIRECTION('ref_axis',(-0.707106781186558,-0.707106781186537,0.));
#7990=DIRECTION('',(0.,0.,1.));
#7991=DIRECTION('',(0.,0.,-1.));
#7992=DIRECTION('center_axis',(1.,0.,0.));
#7993=DIRECTION('ref_axis',(0.,0.,-1.));
#7994=DIRECTION('center_axis',(-1.,0.,0.));
#7995=DIRECTION('ref_axis',(0.,0.,-1.));
#7996=DIRECTION('center_axis',(1.,0.,0.));
#7997=DIRECTION('ref_axis',(0.,0.,-1.));
#7998=DIRECTION('center_axis',(0.,0.,-1.));
#7999=DIRECTION('ref_axis',(0.707106781186516,-0.707106781186579,0.));
#8000=DIRECTION('',(0.,0.,1.));
#8001=DIRECTION('',(0.,0.,-1.));
#8002=DIRECTION('center_axis',(-1.,5.9211894646675E-16,0.));
#8003=DIRECTION('ref_axis',(0.,0.,-1.));
#8004=DIRECTION('center_axis',(-1.,5.9211894646675E-16,0.));
#8005=DIRECTION('ref_axis',(2.62953635073665E-32,4.44089209850053E-17,-1.));
#8006=DIRECTION('center_axis',(1.,-5.9211894646675E-16,0.));
#8007=DIRECTION('ref_axis',(0.,4.44089209850053E-17,-1.));
#8008=DIRECTION('center_axis',(1.,0.,0.));
#8009=DIRECTION('ref_axis',(0.,0.,-1.));
#8010=DIRECTION('center_axis',(1.,0.,0.));
#8011=DIRECTION('ref_axis',(0.,0.,-1.));
#8012=DIRECTION('center_axis',(-1.,0.,0.));
#8013=DIRECTION('ref_axis',(0.,0.,-1.));
#8014=DIRECTION('center_axis',(-1.,5.9211894646675E-16,0.));
#8015=DIRECTION('ref_axis',(0.,0.,-1.));
#8016=DIRECTION('center_axis',(1.,-5.9211894646675E-16,0.));
#8017=DIRECTION('ref_axis',(0.,4.44089209850053E-17,-1.));
#8018=DIRECTION('center_axis',(-1.,5.9211894646675E-16,0.));
#8019=DIRECTION('ref_axis',(2.62953635073665E-32,4.44089209850053E-17,-1.));
#8020=DIRECTION('center_axis',(5.9211894646675E-16,1.,0.));
#8021=DIRECTION('ref_axis',(0.707106781186563,0.,0.707106781186532));
#8022=DIRECTION('',(-5.9211894646675E-16,-1.,0.));
#8023=DIRECTION('',(5.9211894646675E-16,1.,0.));
#8024=DIRECTION('center_axis',(-1.,0.,0.));
#8025=DIRECTION('ref_axis',(0.,0.707106781186547,0.707106781186547));
#8026=DIRECTION('',(1.,0.,0.));
#8027=DIRECTION('',(-1.,0.,0.));
#8028=DIRECTION('center_axis',(0.,-1.,0.));
#8029=DIRECTION('ref_axis',(-0.707106781186563,0.,0.707106781186532));
#8030=DIRECTION('',(0.,1.,0.));
#8031=DIRECTION('',(0.,-1.,0.));
#8032=DIRECTION('center_axis',(1.,0.,0.));
#8033=DIRECTION('ref_axis',(0.,-0.707106781186542,0.707106781186553));
#8034=DIRECTION('',(-1.,0.,0.));
#8035=DIRECTION('',(1.,0.,0.));
#8036=DIRECTION('center_axis',(0.,1.,0.));
#8037=DIRECTION('ref_axis',(-0.707106781186563,0.,0.707106781186532));
#8038=DIRECTION('',(0.,1.,0.));
#8039=DIRECTION('center_axis',(-1.,2.77555756156289E-16,0.));
#8040=DIRECTION('ref_axis',(0.,-0.70710678118654,-0.707106781186555));
#8041=DIRECTION('',(-1.,2.77555756156289E-16,0.));
#8042=DIRECTION('center_axis',(-5.9211894646675E-16,-1.,0.));
#8043=DIRECTION('ref_axis',(0.707106781186521,0.,0.707106781186574));
#8044=DIRECTION('',(-5.9211894646675E-16,-1.,0.));
#8045=DIRECTION('center_axis',(1.,0.,0.));
#8046=DIRECTION('ref_axis',(0.,0.70710678118654,-0.707106781186555));
#8047=DIRECTION('',(1.,0.,0.));
#8048=DIRECTION('center_axis',(0.,-1.,0.));
#8049=DIRECTION('ref_axis',(-0.707106781186563,0.,0.707106781186532));
#8050=DIRECTION('',(0.,1.,0.));
#8051=DIRECTION('center_axis',(0.,0.,-1.));
#8052=DIRECTION('ref_axis',(-0.707106781186568,0.707106781186527,0.));
#8053=DIRECTION('',(0.,0.,1.));
#8054=DIRECTION('',(0.,0.,-1.));
#8055=DIRECTION('center_axis',(5.9211894646675E-16,1.,0.));
#8056=DIRECTION('ref_axis',(0.707106781186563,0.,0.707106781186532));
#8057=DIRECTION('',(-5.9211894646675E-16,-1.,0.));
#8058=DIRECTION('center_axis',(0.,0.,-1.));
#8059=DIRECTION('ref_axis',(0.707106781186516,0.707106781186579,0.));
#8060=DIRECTION('',(0.,0.,1.));
#8061=DIRECTION('',(0.,0.,-1.));
#8062=DIRECTION('center_axis',(1.,0.,0.));
#8063=DIRECTION('ref_axis',(0.,-0.707106781186553,0.707106781186542));
#8064=DIRECTION('',(-1.,0.,0.));
#8065=DIRECTION('center_axis',(-1.,0.,0.));
#8066=DIRECTION('ref_axis',(0.,-0.707106781186547,-0.707106781186547));
#8067=DIRECTION('',(1.,0.,0.));
#8068=DIRECTION('',(-1.,0.,0.));
#8069=DIRECTION('center_axis',(0.,-1.,0.));
#8070=DIRECTION('ref_axis',(0.,0.,1.));
#8071=DIRECTION('',(-1.,0.,0.));
#8072=DIRECTION('center_axis',(-1.,0.,0.));
#8073=DIRECTION('ref_axis',(0.,6.12323399573677E-17,-1.));
#8074=DIRECTION('',(-1.,0.,0.));
#8075=DIRECTION('center_axis',(1.,0.,0.));
#8076=DIRECTION('ref_axis',(0.,-6.12323399573677E-17,-1.));
#8077=DIRECTION('',(-1.,0.,0.));
#8078=DIRECTION('',(-1.,0.,0.));
#8079=DIRECTION('center_axis',(0.,-1.,0.));
#8080=DIRECTION('ref_axis',(0.,0.,1.));
#8081=DIRECTION('center_axis',(0.,0.,1.));
#8082=DIRECTION('ref_axis',(1.,0.,0.));
#8083=DIRECTION('center_axis',(0.,1.,0.));
#8084=DIRECTION('ref_axis',(-1.,0.,0.));
#8085=DIRECTION('center_axis',(0.,1.,0.));
#8086=DIRECTION('ref_axis',(-1.,0.,0.));
#8087=DIRECTION('center_axis',(0.,1.,0.));
#8088=DIRECTION('ref_axis',(-1.,0.,0.));
#8089=DIRECTION('center_axis',(0.,0.,-1.));
#8090=DIRECTION('ref_axis',(-1.,0.,0.));
#8091=DIRECTION('center_axis',(-2.77555756156289E-16,-1.,0.));
#8092=DIRECTION('ref_axis',(1.,-2.77555756156289E-16,0.));
#8093=DIRECTION('center_axis',(0.,0.,-1.));
#8094=DIRECTION('ref_axis',(-1.,0.,0.));
#8095=DIRECTION('center_axis',(-1.,5.9211894646675E-16,0.));
#8096=DIRECTION('ref_axis',(-5.9211894646675E-16,-1.,0.));
#8097=DIRECTION('center_axis',(0.,0.,-1.));
#8098=DIRECTION('ref_axis',(-1.,0.,0.));
#8099=DIRECTION('center_axis',(1.,0.,0.));
#8100=DIRECTION('ref_axis',(0.,1.,0.));
#8101=DIRECTION('center_axis',(0.,1.,0.));
#8102=DIRECTION('ref_axis',(0.,0.,-1.));
#8103=DIRECTION('center_axis',(0.,1.,0.));
#8104=DIRECTION('ref_axis',(0.,0.,-1.));
#8105=DIRECTION('axis',(0.,0.,1.));
#8106=DIRECTION('refdir',(1.,0.,0.));
#8107=DIRECTION('center_axis',(-1.,0.,0.));
#8108=DIRECTION('ref_axis',(0.,-1.,0.));
#8109=DIRECTION('center_axis',(1.,0.,0.));
#8110=DIRECTION('ref_axis',(0.,-1.,0.));
#8111=DIRECTION('center_axis',(-1.,0.,0.));
#8112=DIRECTION('ref_axis',(0.,-1.,0.));
#8113=DIRECTION('center_axis',(1.,0.,0.));
#8114=DIRECTION('ref_axis',(0.,-1.,0.));
#8115=DIRECTION('',(1.,0.,0.));
#8116=DIRECTION('center_axis',(-1.,0.,0.));
#8117=DIRECTION('ref_axis',(0.,-1.,0.));
#8118=DIRECTION('axis',(0.,0.,1.));
#8119=DIRECTION('refdir',(1.,0.,0.));
#8120=DIRECTION('center_axis',(1.,0.,0.));
#8121=DIRECTION('ref_axis',(0.,0.,1.));
#8122=DIRECTION('center_axis',(1.,0.,0.));
#8123=DIRECTION('ref_axis',(0.,-1.,0.));
#8124=DIRECTION('center_axis',(0.,1.,0.));
#8125=DIRECTION('ref_axis',(0.,0.,-1.));
#8126=DIRECTION('center_axis',(-1.,0.,0.));
#8127=DIRECTION('ref_axis',(0.,-1.,0.));
#8128=DIRECTION('center_axis',(-1.,0.,0.));
#8129=DIRECTION('ref_axis',(0.,-1.,0.));
#8130=DIRECTION('center_axis',(-1.,0.,0.));
#8131=DIRECTION('ref_axis',(0.,-1.,0.));
#8132=DIRECTION('center_axis',(-1.,0.,0.));
#8133=DIRECTION('ref_axis',(0.,-1.,0.));
#8134=DIRECTION('center_axis',(1.,0.,0.));
#8135=DIRECTION('ref_axis',(0.,-1.,0.));
#8136=DIRECTION('',(1.,0.,0.));
#8137=DIRECTION('center_axis',(1.,0.,0.));
#8138=DIRECTION('ref_axis',(0.,-1.,0.));
#8139=DIRECTION('center_axis',(1.,0.,0.));
#8140=DIRECTION('ref_axis',(0.,-1.,0.));
#8141=DIRECTION('center_axis',(-1.,0.,0.));
#8142=DIRECTION('ref_axis',(0.,0.,-1.));
#8143=DIRECTION('center_axis',(0.,1.,0.));
#8144=DIRECTION('ref_axis',(0.,0.,1.));
#8145=DIRECTION('center_axis',(1.,0.,0.));
#8146=DIRECTION('ref_axis',(0.,-1.,0.));
#8147=DIRECTION('center_axis',(1.,0.,0.));
#8148=DIRECTION('ref_axis',(0.,-1.,0.));
#8149=DIRECTION('center_axis',(1.,0.,0.));
#8150=DIRECTION('ref_axis',(0.,-1.,0.));
#8151=DIRECTION('',(1.,0.,0.));
#8152=DIRECTION('center_axis',(-1.,0.,0.));
#8153=DIRECTION('ref_axis',(0.,-1.,0.));
#8154=DIRECTION('center_axis',(-1.,0.,0.));
#8155=DIRECTION('ref_axis',(0.,-1.,0.));
#8156=DIRECTION('center_axis',(-1.,0.,0.));
#8157=DIRECTION('ref_axis',(0.,0.,-1.));
#8158=DIRECTION('center_axis',(-1.,0.,0.));
#8159=DIRECTION('ref_axis',(0.,-1.,0.));
#8160=DIRECTION('center_axis',(0.,1.,0.));
#8161=DIRECTION('ref_axis',(0.,0.,1.));
#8162=DIRECTION('center_axis',(-1.,0.,0.));
#8163=DIRECTION('ref_axis',(0.,-1.,0.));
#8164=DIRECTION('center_axis',(1.,0.,0.));
#8165=DIRECTION('ref_axis',(0.,-1.,0.));
#8166=DIRECTION('center_axis',(1.,0.,0.));
#8167=DIRECTION('ref_axis',(0.,0.,1.));
#8168=DIRECTION('center_axis',(0.,1.,0.));
#8169=DIRECTION('ref_axis',(0.,0.,-1.));
#8170=DIRECTION('axis',(0.,0.,1.));
#8171=DIRECTION('refdir',(1.,0.,0.));
#8172=DIRECTION('center_axis',(1.,0.,0.));
#8173=DIRECTION('ref_axis',(0.,1.,0.));
#8174=DIRECTION('center_axis',(1.,0.,0.));
#8175=DIRECTION('ref_axis',(0.,1.,0.));
#8176=DIRECTION('center_axis',(-1.,0.,0.));
#8177=DIRECTION('ref_axis',(0.,1.,0.));
#8178=DIRECTION('center_axis',(-1.,0.,0.));
#8179=DIRECTION('ref_axis',(0.,1.,0.));
#8180=DIRECTION('',(-1.,0.,0.));
#8181=DIRECTION('center_axis',(1.,0.,0.));
#8182=DIRECTION('ref_axis',(0.,1.,0.));
#8183=DIRECTION('axis',(0.,0.,1.));
#8184=DIRECTION('refdir',(1.,0.,0.));
#8185=DIRECTION('center_axis',(-1.,0.,0.));
#8186=DIRECTION('ref_axis',(0.,-1.,0.));
#8187=DIRECTION('center_axis',(-1.,0.,0.));
#8188=DIRECTION('ref_axis',(0.,-1.,0.));
#8189=DIRECTION('center_axis',(1.,0.,0.));
#8190=DIRECTION('ref_axis',(0.,-1.,0.));
#8191=DIRECTION('center_axis',(1.,0.,0.));
#8192=DIRECTION('ref_axis',(0.,-1.,0.));
#8193=DIRECTION('',(-1.,0.,0.));
#8194=DIRECTION('center_axis',(-1.,0.,0.));
#8195=DIRECTION('ref_axis',(0.,-1.,0.));
#8196=DIRECTION('axis',(0.,0.,1.));
#8197=DIRECTION('refdir',(1.,0.,0.));
#8198=DIRECTION('center_axis',(-1.,0.,0.));
#8199=DIRECTION('ref_axis',(0.,0.,1.));
#8200=DIRECTION('center_axis',(1.,0.,0.));
#8201=DIRECTION('ref_axis',(0.,-1.,0.));
#8202=DIRECTION('center_axis',(0.,-1.,0.));
#8203=DIRECTION('ref_axis',(0.,0.,-1.));
#8204=DIRECTION('center_axis',(-1.,0.,0.));
#8205=DIRECTION('ref_axis',(0.,-1.,0.));
#8206=DIRECTION('center_axis',(-1.,0.,0.));
#8207=DIRECTION('ref_axis',(0.,-1.,0.));
#8208=DIRECTION('center_axis',(-1.,0.,0.));
#8209=DIRECTION('ref_axis',(0.,-1.,0.));
#8210=DIRECTION('center_axis',(-1.,0.,0.));
#8211=DIRECTION('ref_axis',(0.,-1.,0.));
#8212=DIRECTION('center_axis',(1.,0.,0.));
#8213=DIRECTION('ref_axis',(0.,-1.,0.));
#8214=DIRECTION('',(-1.,0.,0.));
#8215=DIRECTION('center_axis',(1.,0.,0.));
#8216=DIRECTION('ref_axis',(0.,-1.,0.));
#8217=DIRECTION('center_axis',(1.,0.,0.));
#8218=DIRECTION('ref_axis',(0.,-1.,0.));
#8219=DIRECTION('center_axis',(1.,0.,0.));
#8220=DIRECTION('ref_axis',(0.,0.,-1.));
#8221=DIRECTION('center_axis',(0.,-1.,0.));
#8222=DIRECTION('ref_axis',(0.,0.,1.));
#8223=DIRECTION('center_axis',(1.,0.,0.));
#8224=DIRECTION('ref_axis',(0.,-1.,0.));
#8225=DIRECTION('center_axis',(1.,0.,0.));
#8226=DIRECTION('ref_axis',(0.,-1.,0.));
#8227=DIRECTION('center_axis',(1.,0.,0.));
#8228=DIRECTION('ref_axis',(0.,-1.,0.));
#8229=DIRECTION('',(-1.,0.,0.));
#8230=DIRECTION('center_axis',(-1.,0.,0.));
#8231=DIRECTION('ref_axis',(0.,-1.,0.));
#8232=DIRECTION('center_axis',(-1.,0.,0.));
#8233=DIRECTION('ref_axis',(0.,-1.,0.));
#8234=DIRECTION('center_axis',(1.,0.,0.));
#8235=DIRECTION('ref_axis',(0.,0.,-1.));
#8236=DIRECTION('center_axis',(-1.,0.,0.));
#8237=DIRECTION('ref_axis',(0.,-1.,0.));
#8238=DIRECTION('center_axis',(0.,-1.,0.));
#8239=DIRECTION('ref_axis',(0.,0.,1.));
#8240=DIRECTION('center_axis',(-1.,0.,0.));
#8241=DIRECTION('ref_axis',(0.,-1.,0.));
#8242=DIRECTION('center_axis',(1.,0.,0.));
#8243=DIRECTION('ref_axis',(0.,-1.,0.));
#8244=DIRECTION('center_axis',(-1.,0.,0.));
#8245=DIRECTION('ref_axis',(0.,0.,1.));
#8246=DIRECTION('center_axis',(0.,-1.,0.));
#8247=DIRECTION('ref_axis',(0.,0.,-1.));
#8248=DIRECTION('axis',(0.,0.,1.));
#8249=DIRECTION('refdir',(1.,0.,0.));
#8250=DIRECTION('center_axis',(0.,0.,1.));
#8251=DIRECTION('ref_axis',(1.,0.,0.));
#8252=DIRECTION('center_axis',(0.,0.,-1.));
#8253=DIRECTION('ref_axis',(1.,0.,0.));
#8254=DIRECTION('center_axis',(0.,-1.,0.));
#8255=DIRECTION('ref_axis',(-1.,0.,0.));
#8256=DIRECTION('center_axis',(0.,0.,1.));
#8257=DIRECTION('ref_axis',(1.,0.,0.));
#8258=DIRECTION('center_axis',(0.,0.,1.));
#8259=DIRECTION('ref_axis',(1.,0.,0.));
#8260=DIRECTION('',(1.,0.,0.));
#8261=DIRECTION('',(-5.9211894646675E-16,1.,0.));
#8262=DIRECTION('',(-1.,-2.77555756156289E-16,0.));
#8263=DIRECTION('',(0.,-1.,0.));
#8264=DIRECTION('center_axis',(0.,0.,1.));
#8265=DIRECTION('ref_axis',(1.,0.,0.));
#8266=DIRECTION('center_axis',(0.,0.,-1.));
#8267=DIRECTION('ref_axis',(1.,0.,0.));
#8268=DIRECTION('',(0.,0.,-1.));
#8269=DIRECTION('center_axis',(0.,0.,-1.));
#8270=DIRECTION('ref_axis',(1.,0.,0.));
#8271=DIRECTION('center_axis',(0.,0.,1.));
#8272=DIRECTION('ref_axis',(1.,0.,0.));
#8273=DIRECTION('center_axis',(0.,0.,-1.));
#8274=DIRECTION('ref_axis',(1.,0.,0.));
#8275=DIRECTION('center_axis',(0.,-1.,0.));
#8276=DIRECTION('ref_axis',(-1.,0.,0.));
#8277=DIRECTION('center_axis',(0.,0.,-1.));
#8278=DIRECTION('ref_axis',(1.,0.,0.));
#8279=DIRECTION('',(0.,0.,-1.));
#8280=DIRECTION('center_axis',(0.,0.,-1.));
#8281=DIRECTION('ref_axis',(1.,0.,0.));
#8282=DIRECTION('center_axis',(0.,0.,-1.));
#8283=DIRECTION('ref_axis',(-1.,0.,0.));
#8284=DIRECTION('center_axis',(0.,0.,1.));
#8285=DIRECTION('ref_axis',(1.,0.,0.));
#8286=DIRECTION('center_axis',(0.,-1.,0.));
#8287=DIRECTION('ref_axis',(1.,0.,0.));
#8288=DIRECTION('center_axis',(0.,0.,-1.));
#8289=DIRECTION('ref_axis',(1.,0.,0.));
#8290=DIRECTION('center_axis',(0.,0.,-1.));
#8291=DIRECTION('ref_axis',(1.,0.,0.));
#8292=DIRECTION('center_axis',(0.,0.,-1.));
#8293=DIRECTION('ref_axis',(1.,0.,0.));
#8294=DIRECTION('',(1.,0.,0.));
#8295=DIRECTION('',(-5.9211894646675E-16,1.,0.));
#8296=DIRECTION('',(-1.,0.,0.));
#8297=DIRECTION('',(0.,-1.,0.));
#8298=DIRECTION('center_axis',(0.,0.,1.));
#8299=DIRECTION('ref_axis',(1.,0.,0.));
#8300=DIRECTION('center_axis',(0.,0.,1.));
#8301=DIRECTION('ref_axis',(1.,0.,0.));
#8302=DIRECTION('',(0.,0.,-1.));
#8303=DIRECTION('center_axis',(0.,0.,1.));
#8304=DIRECTION('ref_axis',(1.,0.,0.));
#8305=DIRECTION('center_axis',(0.,0.,-1.));
#8306=DIRECTION('ref_axis',(-1.,0.,0.));
#8307=DIRECTION('center_axis',(0.,-1.,0.));
#8308=DIRECTION('ref_axis',(1.,0.,0.));
#8309=DIRECTION('center_axis',(0.,0.,-1.));
#8310=DIRECTION('ref_axis',(1.,0.,0.));
#8311=DIRECTION('center_axis',(0.,0.,-1.));
#8312=DIRECTION('ref_axis',(1.,0.,0.));
#8313=DIRECTION('center_axis',(0.,0.,1.));
#8314=DIRECTION('ref_axis',(1.,0.,0.));
#8315=DIRECTION('',(0.,0.,-1.));
#8316=DIRECTION('center_axis',(0.,0.,1.));
#8317=DIRECTION('ref_axis',(1.,0.,0.));
#8318=DIRECTION('center_axis',(0.408248290463861,0.408248290463837,-0.81649658092774));
#8319=DIRECTION('ref_axis',(-0.577350269189669,-0.577350269189598,-0.57735026918961));
#8320=DIRECTION('center_axis',(0.,-7.40148683083442E-15,-1.));
#8321=DIRECTION('ref_axis',(-1.,0.,0.));
#8322=DIRECTION('center_axis',(0.,-1.,0.));
#8323=DIRECTION('ref_axis',(0.,0.,-1.));
#8324=DIRECTION('center_axis',(-1.,0.,-5.92118946466745E-14));
#8325=DIRECTION('ref_axis',(0.,-1.,0.));
#8326=DIRECTION('center_axis',(-0.408248290463865,-0.81649658092773,0.408248290463853));
#8327=DIRECTION('ref_axis',(0.577350269189602,-0.577350269189626,-0.577350269189649));
#8328=DIRECTION('center_axis',(1.,0.,0.));
#8329=DIRECTION('ref_axis',(0.,0.,-1.));
#8330=DIRECTION('center_axis',(0.,-1.,-2.96059473233375E-14));
#8331=DIRECTION('ref_axis',(1.,0.,0.));
#8332=DIRECTION('center_axis',(-7.40148683083454E-15,0.,-1.));
#8333=DIRECTION('ref_axis',(0.,-1.,0.));
#8334=DIRECTION('center_axis',(-0.816496580927716,-0.408248290463882,0.408248290463864));
#8335=DIRECTION('ref_axis',(-0.577350269189634,0.577350269189634,-0.57735026918961));
#8336=DIRECTION('center_axis',(-1.,0.,0.));
#8337=DIRECTION('ref_axis',(0.,0.,-1.));
#8338=DIRECTION('center_axis',(0.,1.,0.));
#8339=DIRECTION('ref_axis',(-1.,0.,0.));
#8340=DIRECTION('center_axis',(0.,0.,-1.));
#8341=DIRECTION('ref_axis',(0.,1.,0.));
#8342=DIRECTION('center_axis',(-5.9211894646675E-16,1.,0.));
#8343=DIRECTION('ref_axis',(-0.707106781186563,0.,-0.707106781186532));
#8344=DIRECTION('',(5.9211894646675E-16,-1.,0.));
#8345=DIRECTION('',(-5.9211894646675E-16,1.,0.));
#8346=DIRECTION('center_axis',(-0.816496580927728,0.408248290463864,-0.408248290463858));
#8347=DIRECTION('ref_axis',(-0.577350269189594,-0.577350269189642,0.577350269189642));
#8348=DIRECTION('center_axis',(0.,-1.,0.));
#8349=DIRECTION('ref_axis',(-1.,0.,0.));
#8350=DIRECTION('center_axis',(-7.40148683083454E-15,0.,1.));
#8351=DIRECTION('ref_axis',(0.,-1.,0.));
#8352=DIRECTION('center_axis',(-1.,0.,0.));
#8353=DIRECTION('ref_axis',(0.,0.,1.));
#8354=DIRECTION('center_axis',(0.,0.,1.));
#8355=DIRECTION('ref_axis',(-0.707106781186516,-0.707106781186579,0.));
#8356=DIRECTION('',(0.,0.,-1.));
#8357=DIRECTION('',(0.,0.,1.));
#8358=DIRECTION('center_axis',(0.408248290463855,-0.816496580927734,-0.408248290463855));
#8359=DIRECTION('ref_axis',(0.577350269189651,0.577350269189604,-0.577350269189622));
#8360=DIRECTION('center_axis',(0.,0.,-1.));
#8361=DIRECTION('ref_axis',(1.,0.,0.));
#8362=DIRECTION('center_axis',(0.,1.,0.));
#8363=DIRECTION('ref_axis',(0.,0.,-1.));
#8364=DIRECTION('center_axis',(1.,0.,0.));
#8365=DIRECTION('ref_axis',(0.,1.,0.));
#8366=DIRECTION('center_axis',(0.,1.,0.));
#8367=DIRECTION('ref_axis',(0.707106781186563,0.,-0.707106781186532));
#8368=DIRECTION('',(0.,-1.,0.));
#8369=DIRECTION('',(0.,1.,0.));
#8370=DIRECTION('center_axis',(-1.,0.,0.));
#8371=DIRECTION('ref_axis',(0.,0.707106781186553,-0.707106781186542));
#8372=DIRECTION('',(1.,0.,0.));
#8373=DIRECTION('',(-1.,0.,0.));
#8374=DIRECTION('center_axis',(-0.408248290463864,-0.816496580927728,-0.408248290463858));
#8375=DIRECTION('ref_axis',(0.5773502691896,-0.577350269189624,0.577350269189653));
#8376=DIRECTION('center_axis',(1.,0.,0.));
#8377=DIRECTION('ref_axis',(0.,-1.,0.));
#8378=DIRECTION('center_axis',(0.,7.40148683083454E-15,1.));
#8379=DIRECTION('ref_axis',(1.,0.,0.));
#8380=DIRECTION('center_axis',(-1.48029736616691E-14,-1.,0.));
#8381=DIRECTION('ref_axis',(0.,0.,1.));
#8382=DIRECTION('center_axis',(0.,0.,1.));
#8383=DIRECTION('ref_axis',(0.707106781186568,-0.707106781186527,0.));
#8384=DIRECTION('',(0.,0.,-1.));
#8385=DIRECTION('',(0.,0.,1.));
#8386=DIRECTION('center_axis',(-0.408248290463856,-0.816496580927712,0.408248290463898));
#8387=DIRECTION('ref_axis',(-0.577350269189574,0.577350269189645,0.577350269189657));
#8388=DIRECTION('center_axis',(0.,0.,1.));
#8389=DIRECTION('ref_axis',(-1.,0.,0.));
#8390=DIRECTION('center_axis',(-1.48029736616699E-14,1.,0.));
#8391=DIRECTION('ref_axis',(0.,0.,1.));
#8392=DIRECTION('center_axis',(-1.,0.,-5.9211894646675E-14));
#8393=DIRECTION('ref_axis',(0.,1.,0.));
#8394=DIRECTION('center_axis',(1.,0.,0.));
#8395=DIRECTION('ref_axis',(0.,0.,-1.));
#8396=DIRECTION('center_axis',(1.,0.,0.));
#8397=DIRECTION('ref_axis',(0.,1.,0.));
#8398=DIRECTION('center_axis',(0.,0.,1.));
#8399=DIRECTION('ref_axis',(-1.,0.,0.));
#8400=DIRECTION('center_axis',(-1.,-5.9211894646675E-16,0.));
#8401=DIRECTION('ref_axis',(0.,0.707106781186545,-0.70710678118655));
#8402=DIRECTION('center_axis',(0.,-1.,0.));
#8403=DIRECTION('ref_axis',(0.,0.,1.));
#8404=DIRECTION('center_axis',(0.408248290463862,-0.816496580927724,0.408248290463868));
#8405=DIRECTION('ref_axis',(0.57735026918959,0.577350269189638,0.577350269189649));
#8406=DIRECTION('center_axis',(0.,0.,1.));
#8407=DIRECTION('ref_axis',(0.,1.,0.));
#8408=DIRECTION('center_axis',(1.,0.,0.));
#8409=DIRECTION('ref_axis',(0.,0.,1.));
#8410=DIRECTION('center_axis',(0.,1.,0.));
#8411=DIRECTION('ref_axis',(1.,0.,0.));
#8412=DIRECTION('center_axis',(1.,0.,0.));
#8413=DIRECTION('ref_axis',(0.,0.707106781186542,0.707106781186553));
#8414=DIRECTION('',(-1.,0.,0.));
#8415=DIRECTION('center_axis',(1.,0.,0.));
#8416=DIRECTION('ref_axis',(0.,0.,-1.));
#8417=DIRECTION('center_axis',(1.,0.,0.));
#8418=DIRECTION('ref_axis',(0.,0.707106781186545,-0.70710678118655));
#8419=DIRECTION('center_axis',(0.,0.,1.));
#8420=DIRECTION('ref_axis',(0.,-1.,0.));
#8421=DIRECTION('center_axis',(-1.,0.,0.));
#8422=DIRECTION('ref_axis',(0.,0.,-1.));
#8423=DIRECTION('center_axis',(0.,-1.,0.));
#8424=DIRECTION('ref_axis',(1.,0.,0.));
#8425=DIRECTION('center_axis',(-1.,0.,0.));
#8426=DIRECTION('ref_axis',(0.,0.,1.));
#8427=DIRECTION('center_axis',(-1.,-5.9211894646675E-16,0.));
#8428=DIRECTION('ref_axis',(0.,-0.70710678118654,-0.707106781186555));
#8429=DIRECTION('center_axis',(0.,0.,1.));
#8430=DIRECTION('ref_axis',(0.,1.,0.));
#8431=DIRECTION('center_axis',(1.,5.92118946466763E-14,0.));
#8432=DIRECTION('ref_axis',(0.,0.,-1.));
#8433=DIRECTION('center_axis',(0.,1.,0.));
#8434=DIRECTION('ref_axis',(-1.,0.,0.));
#8435=DIRECTION('center_axis',(0.408248290463862,-0.816496580927724,-0.408248290463868));
#8436=DIRECTION('ref_axis',(-0.577350269189592,-0.577350269189639,0.577350269189645));
#8437=DIRECTION('center_axis',(0.,-1.,0.));
#8438=DIRECTION('ref_axis',(-1.,0.,0.));
#8439=DIRECTION('center_axis',(0.,0.,1.));
#8440=DIRECTION('ref_axis',(0.,-1.,0.));
#8441=DIRECTION('center_axis',(-1.,5.92118946466754E-14,0.));
#8442=DIRECTION('ref_axis',(0.,0.,1.));
#8443=DIRECTION('center_axis',(0.,0.,-1.));
#8444=DIRECTION('ref_axis',(-0.707106781186527,-0.707106781186568,0.));
#8445=DIRECTION('',(0.,0.,1.));
#8446=DIRECTION('',(0.,0.,-1.));
#8447=DIRECTION('center_axis',(-1.,0.,0.));
#8448=DIRECTION('ref_axis',(0.,0.,1.));
#8449=DIRECTION('center_axis',(-1.,0.,0.));
#8450=DIRECTION('ref_axis',(0.,-1.,0.));
#8451=DIRECTION('center_axis',(0.,0.,1.));
#8452=DIRECTION('ref_axis',(1.,0.,0.));
#8453=DIRECTION('center_axis',(1.,0.,0.));
#8454=DIRECTION('ref_axis',(0.,-0.70710678118654,-0.707106781186555));
#8455=DIRECTION('center_axis',(0.,1.,0.));
#8456=DIRECTION('ref_axis',(0.,0.,1.));
#8457=DIRECTION('center_axis',(-0.408248290463867,-0.816496580927722,-0.408248290463867));
#8458=DIRECTION('ref_axis',(0.5773502691896,-0.577350269189636,0.577350269189642));
#8459=DIRECTION('center_axis',(1.,0.,0.));
#8460=DIRECTION('ref_axis',(0.,-1.,0.));
#8461=DIRECTION('center_axis',(0.,0.,1.));
#8462=DIRECTION('ref_axis',(1.,0.,0.));
#8463=DIRECTION('center_axis',(0.,-1.,0.));
#8464=DIRECTION('ref_axis',(0.,0.,1.));
#8465=DIRECTION('center_axis',(0.,0.,1.));
#8466=DIRECTION('ref_axis',(0.707106781186568,-0.707106781186527,0.));
#8467=DIRECTION('',(0.,0.,-1.));
#8468=DIRECTION('',(0.,0.,1.));
#8469=DIRECTION('center_axis',(-0.408248290463866,-0.81649658092772,0.408248290463872));
#8470=DIRECTION('ref_axis',(-0.577350269189592,0.577350269189628,0.577350269189657));
#8471=DIRECTION('center_axis',(-1.,0.,5.9211894646675E-14));
#8472=DIRECTION('ref_axis',(0.,1.,0.));
#8473=DIRECTION('center_axis',(0.,0.,1.));
#8474=DIRECTION('ref_axis',(-1.,0.,0.));
#8475=DIRECTION('center_axis',(1.48029736616682E-14,1.,0.));
#8476=DIRECTION('ref_axis',(0.,0.,1.));
#8477=DIRECTION('center_axis',(0.,0.,1.));
#8478=DIRECTION('ref_axis',(-0.707106781186527,0.707106781186568,0.));
#8479=DIRECTION('',(0.,0.,-1.));
#8480=DIRECTION('',(0.,0.,1.));
#8481=DIRECTION('center_axis',(-0.408248290463859,0.408248290463847,-0.816496580927736));
#8482=DIRECTION('ref_axis',(-0.577350269189657,0.577350269189622,0.577350269189598));
#8483=DIRECTION('center_axis',(0.,7.40148683083442E-15,1.));
#8484=DIRECTION('ref_axis',(-1.,0.,0.));
#8485=DIRECTION('center_axis',(0.,1.,0.));
#8486=DIRECTION('ref_axis',(0.,0.,1.));
#8487=DIRECTION('center_axis',(-1.,0.,0.));
#8488=DIRECTION('ref_axis',(0.,1.,0.));
#8489=DIRECTION('center_axis',(5.9211894646675E-16,-1.,0.));
#8490=DIRECTION('ref_axis',(-0.707106781186563,0.,0.707106781186532));
#8491=DIRECTION('',(-5.9211894646675E-16,1.,0.));
#8492=DIRECTION('',(5.9211894646675E-16,-1.,0.));
#8493=DIRECTION('center_axis',(0.408248290463865,-0.81649658092773,0.408248290463853));
#8494=DIRECTION('ref_axis',(0.5773502691896,0.577350269189624,0.577350269189653));
#8495=DIRECTION('center_axis',(0.,1.,2.96059473233375E-14));
#8496=DIRECTION('ref_axis',(1.,0.,0.));
#8497=DIRECTION('center_axis',(0.,0.,1.));
#8498=DIRECTION('ref_axis',(0.,1.,0.));
#8499=DIRECTION('center_axis',(1.,0.,0.));
#8500=DIRECTION('ref_axis',(0.,0.,1.));
#8501=DIRECTION('center_axis',(0.,0.,1.));
#8502=DIRECTION('ref_axis',(0.707106781186568,0.707106781186527,0.));
#8503=DIRECTION('',(0.,0.,-1.));
#8504=DIRECTION('',(0.,0.,1.));
#8505=DIRECTION('center_axis',(-1.,-2.77555756156289E-16,0.));
#8506=DIRECTION('ref_axis',(0.,0.707106781186553,0.707106781186542));
#8507=DIRECTION('',(1.,2.77555756156289E-16,0.));
#8508=DIRECTION('',(-1.,-2.77555756156289E-16,0.));
#8509=DIRECTION('center_axis',(0.408248290463862,-0.816496580927724,0.408248290463868));
#8510=DIRECTION('ref_axis',(0.57735026918959,0.577350269189638,0.577350269189649));
#8511=DIRECTION('center_axis',(0.,1.,0.));
#8512=DIRECTION('ref_axis',(1.,0.,0.));
#8513=DIRECTION('center_axis',(-7.40148683083454E-15,0.,1.));
#8514=DIRECTION('ref_axis',(0.,1.,0.));
#8515=DIRECTION('center_axis',(1.,0.,0.));
#8516=DIRECTION('ref_axis',(0.,0.,1.));
#8517=DIRECTION('center_axis',(-0.408248290463859,-0.408248290463835,-0.816496580927742));
#8518=DIRECTION('ref_axis',(-0.577350269189663,-0.577350269189604,0.57735026918961));
#8519=DIRECTION('center_axis',(7.40148683083454E-15,0.,1.));
#8520=DIRECTION('ref_axis',(0.,-1.,0.));
#8521=DIRECTION('center_axis',(-1.,5.92118946466754E-14,0.));
#8522=DIRECTION('ref_axis',(0.,0.,1.));
#8523=DIRECTION('center_axis',(0.,-1.,0.));
#8524=DIRECTION('ref_axis',(-1.,0.,0.));
#8525=DIRECTION('center_axis',(0.,0.,-1.));
#8526=DIRECTION('ref_axis',(-0.707106781186516,0.707106781186579,0.));
#8527=DIRECTION('',(0.,0.,1.));
#8528=DIRECTION('',(0.,0.,-1.));
#8529=DIRECTION('center_axis',(-0.816496580927732,-0.408248290463866,0.408248290463848));
#8530=DIRECTION('ref_axis',(0.577350269189588,-0.577350269189659,0.57735026918963));
#8531=DIRECTION('center_axis',(0.,-7.40148683083454E-15,1.));
#8532=DIRECTION('ref_axis',(1.,0.,0.));
#8533=DIRECTION('center_axis',(-2.96059473233381E-14,-1.,0.));
#8534=DIRECTION('ref_axis',(0.,0.,1.));
#8535=DIRECTION('center_axis',(1.,0.,0.));
#8536=DIRECTION('ref_axis',(0.,-1.,0.));
#8537=DIRECTION('center_axis',(0.,1.,0.));
#8538=DIRECTION('ref_axis',(0.707106781186563,0.,0.707106781186532));
#8539=DIRECTION('',(0.,-1.,0.));
#8540=DIRECTION('',(0.,1.,0.));
#8541=DIRECTION('center_axis',(1.,0.,0.));
#8542=DIRECTION('ref_axis',(0.,-0.707106781186547,0.707106781186547));
#8543=DIRECTION('',(-1.,0.,0.));
#8544=DIRECTION('',(1.,0.,0.));
#8545=DIRECTION('center_axis',(0.,0.,1.));
#8546=DIRECTION('ref_axis',(0.707106781186558,0.707106781186537,0.));
#8547=DIRECTION('',(0.,0.,1.));
#8548=DIRECTION('',(0.,0.,-1.));
#8549=DIRECTION('center_axis',(0.,0.,1.));
#8550=DIRECTION('ref_axis',(-0.707106781186516,-0.707106781186579,0.));
#8551=DIRECTION('',(0.,0.,1.));
#8552=DIRECTION('',(0.,0.,-1.));
#8553=DIRECTION('center_axis',(0.,0.,-1.));
#8554=DIRECTION('ref_axis',(0.707106781186568,-0.707106781186527,0.));
#8555=DIRECTION('',(0.,0.,1.));
#8556=DIRECTION('',(0.,0.,-1.));
#8557=DIRECTION('center_axis',(-0.816496580927728,0.408248290463864,-0.408248290463858));
#8558=DIRECTION('ref_axis',(-0.577350269189588,-0.577350269189647,0.577350269189642));
#8559=DIRECTION('center_axis',(0.,0.,1.));
#8560=DIRECTION('ref_axis',(0.,-1.,0.));
#8561=DIRECTION('center_axis',(-1.,0.,0.));
#8562=DIRECTION('ref_axis',(0.,0.,1.));
#8563=DIRECTION('center_axis',(0.,-1.,0.));
#8564=DIRECTION('ref_axis',(-1.,0.,0.));
#8565=DIRECTION('center_axis',(-0.408248290463857,-0.816496580927726,-0.408248290463869));
#8566=DIRECTION('ref_axis',(0.57735026918959,-0.577350269189638,0.577350269189649));
#8567=DIRECTION('center_axis',(0.,0.,1.));
#8568=DIRECTION('ref_axis',(1.,0.,0.));
#8569=DIRECTION('center_axis',(0.,-1.,0.));
#8570=DIRECTION('ref_axis',(0.,0.,1.));
#8571=DIRECTION('center_axis',(1.,0.,0.));
#8572=DIRECTION('ref_axis',(0.,-1.,0.));
#8573=DIRECTION('center_axis',(-0.408248290463861,0.408248290463837,-0.81649658092774));
#8574=DIRECTION('ref_axis',(-0.577350269189665,0.577350269189606,0.577350269189606));
#8575=DIRECTION('center_axis',(0.,0.,1.));
#8576=DIRECTION('ref_axis',(-1.,0.,0.));
#8577=DIRECTION('center_axis',(0.,1.,0.));
#8578=DIRECTION('ref_axis',(0.,0.,1.));
#8579=DIRECTION('center_axis',(-1.,0.,5.9211894646675E-14));
#8580=DIRECTION('ref_axis',(0.,1.,0.));
#8581=DIRECTION('center_axis',(5.9211894646675E-16,-1.,0.));
#8582=DIRECTION('ref_axis',(-0.707106781186563,0.,0.707106781186532));
#8583=DIRECTION('',(-5.9211894646675E-16,1.,0.));
#8584=DIRECTION('',(5.9211894646675E-16,-1.,0.));
#8585=DIRECTION('center_axis',(0.408248290463868,-0.816496580927724,0.408248290463862));
#8586=DIRECTION('ref_axis',(0.577350269189598,0.577350269189634,0.577350269189645));
#8587=DIRECTION('center_axis',(0.,1.,0.));
#8588=DIRECTION('ref_axis',(1.,0.,0.));
#8589=DIRECTION('center_axis',(0.,0.,1.));
#8590=DIRECTION('ref_axis',(0.,1.,0.));
#8591=DIRECTION('center_axis',(1.,0.,0.));
#8592=DIRECTION('ref_axis',(0.,0.,1.));
#8593=DIRECTION('center_axis',(0.,0.,1.));
#8594=DIRECTION('ref_axis',(0.707106781186568,0.707106781186527,0.));
#8595=DIRECTION('',(0.,0.,1.));
#8596=DIRECTION('',(0.,0.,-1.));
#8597=DIRECTION('center_axis',(-1.,0.,0.));
#8598=DIRECTION('ref_axis',(0.,0.707106781186553,0.707106781186542));
#8599=DIRECTION('',(1.,0.,0.));
#8600=DIRECTION('',(-1.,0.,0.));
#8601=DIRECTION('center_axis',(0.,1.,0.));
#8602=DIRECTION('ref_axis',(0.707106781186563,0.,0.707106781186532));
#8603=DIRECTION('',(0.,-1.,0.));
#8604=DIRECTION('',(0.,1.,0.));
#8605=DIRECTION('center_axis',(0.,0.,-1.));
#8606=DIRECTION('ref_axis',(-0.707106781186516,0.707106781186579,0.));
#8607=DIRECTION('',(0.,0.,1.));
#8608=DIRECTION('',(0.,0.,-1.));
#8609=DIRECTION('center_axis',(1.,0.,0.));
#8610=DIRECTION('ref_axis',(0.,-0.707106781186553,0.707106781186542));
#8611=DIRECTION('',(-1.,0.,0.));
#8612=DIRECTION('',(1.,0.,0.));
#8613=DIRECTION('center_axis',(0.,0.,-1.));
#8614=DIRECTION('ref_axis',(0.707106781186558,-0.707106781186537,0.));
#8615=DIRECTION('',(0.,0.,1.));
#8616=DIRECTION('',(0.,0.,-1.));
#8617=DIRECTION('center_axis',(-1.,0.,0.));
#8618=DIRECTION('ref_axis',(0.,0.,-1.));
#8619=DIRECTION('center_axis',(-1.,0.,0.));
#8620=DIRECTION('ref_axis',(0.,0.,-1.));
#8621=DIRECTION('center_axis',(1.,0.,0.));
#8622=DIRECTION('ref_axis',(0.,0.,-1.));
#8623=DIRECTION('center_axis',(0.,0.,1.));
#8624=DIRECTION('ref_axis',(-0.707106781186516,-0.707106781186579,0.));
#8625=DIRECTION('',(0.,0.,1.));
#8626=DIRECTION('',(0.,0.,-1.));
#8627=DIRECTION('center_axis',(1.,5.9211894646675E-16,0.));
#8628=DIRECTION('ref_axis',(0.,0.,-1.));
#8629=DIRECTION('center_axis',(-1.,-5.9211894646675E-16,0.));
#8630=DIRECTION('ref_axis',(-2.62953635073665E-32,4.44089209850053E-17,
-1.));
#8631=DIRECTION('center_axis',(1.,5.9211894646675E-16,0.));
#8632=DIRECTION('ref_axis',(0.,4.44089209850053E-17,-1.));
#8633=DIRECTION('center_axis',(-1.,0.,0.));
#8634=DIRECTION('ref_axis',(0.,0.,-1.));
#8635=DIRECTION('center_axis',(1.,0.,0.));
#8636=DIRECTION('ref_axis',(0.,0.,-1.));
#8637=DIRECTION('center_axis',(-1.,0.,0.));
#8638=DIRECTION('ref_axis',(0.,0.,-1.));
#8639=DIRECTION('center_axis',(1.,5.9211894646675E-16,0.));
#8640=DIRECTION('ref_axis',(0.,0.,-1.));
#8641=DIRECTION('center_axis',(1.,5.9211894646675E-16,0.));
#8642=DIRECTION('ref_axis',(0.,4.44089209850053E-17,-1.));
#8643=DIRECTION('center_axis',(-1.,-5.9211894646675E-16,0.));
#8644=DIRECTION('ref_axis',(-2.62953635073665E-32,4.44089209850053E-17,
-1.));
#8645=DIRECTION('center_axis',(5.9211894646675E-16,-1.,0.));
#8646=DIRECTION('ref_axis',(-0.707106781186563,0.,0.707106781186532));
#8647=DIRECTION('',(-5.9211894646675E-16,1.,0.));
#8648=DIRECTION('',(5.9211894646675E-16,-1.,0.));
#8649=DIRECTION('center_axis',(-1.,0.,0.));
#8650=DIRECTION('ref_axis',(0.,0.707106781186547,0.707106781186547));
#8651=DIRECTION('',(1.,0.,0.));
#8652=DIRECTION('',(-1.,0.,0.));
#8653=DIRECTION('center_axis',(0.,1.,0.));
#8654=DIRECTION('ref_axis',(0.707106781186563,0.,0.707106781186532));
#8655=DIRECTION('',(0.,-1.,0.));
#8656=DIRECTION('',(0.,1.,0.));
#8657=DIRECTION('center_axis',(1.,0.,0.));
#8658=DIRECTION('ref_axis',(0.,-0.707106781186542,0.707106781186553));
#8659=DIRECTION('',(-1.,0.,0.));
#8660=DIRECTION('',(1.,0.,0.));
#8661=DIRECTION('center_axis',(0.,-1.,0.));
#8662=DIRECTION('ref_axis',(0.707106781186563,0.,0.707106781186532));
#8663=DIRECTION('',(0.,1.,0.));
#8664=DIRECTION('center_axis',(-1.,-2.77555756156289E-16,0.));
#8665=DIRECTION('ref_axis',(0.,-0.70710678118654,-0.707106781186555));
#8666=DIRECTION('',(1.,2.77555756156289E-16,0.));
#8667=DIRECTION('center_axis',(-5.9211894646675E-16,1.,0.));
#8668=DIRECTION('ref_axis',(-0.707106781186521,0.,0.707106781186574));
#8669=DIRECTION('',(5.9211894646675E-16,-1.,0.));
#8670=DIRECTION('center_axis',(1.,0.,0.));
#8671=DIRECTION('ref_axis',(0.,0.70710678118654,-0.707106781186555));
#8672=DIRECTION('',(-1.,0.,0.));
#8673=DIRECTION('center_axis',(0.,1.,0.));
#8674=DIRECTION('ref_axis',(0.707106781186563,0.,0.707106781186532));
#8675=DIRECTION('',(0.,1.,0.));
#8676=DIRECTION('center_axis',(0.,0.,1.));
#8677=DIRECTION('ref_axis',(0.707106781186568,0.707106781186527,0.));
#8678=DIRECTION('',(0.,0.,-1.));
#8679=DIRECTION('',(0.,0.,1.));
#8680=DIRECTION('center_axis',(5.9211894646675E-16,-1.,0.));
#8681=DIRECTION('ref_axis',(-0.707106781186563,0.,0.707106781186532));
#8682=DIRECTION('',(5.9211894646675E-16,-1.,0.));
#8683=DIRECTION('center_axis',(0.,0.,1.));
#8684=DIRECTION('ref_axis',(-0.707106781186516,0.707106781186579,0.));
#8685=DIRECTION('',(0.,0.,-1.));
#8686=DIRECTION('',(0.,0.,1.));
#8687=DIRECTION('center_axis',(1.,0.,0.));
#8688=DIRECTION('ref_axis',(0.,-0.707106781186553,0.707106781186542));
#8689=DIRECTION('',(1.,0.,0.));
#8690=DIRECTION('center_axis',(-1.,0.,0.));
#8691=DIRECTION('ref_axis',(0.,-0.707106781186547,-0.707106781186547));
#8692=DIRECTION('',(1.,0.,0.));
#8693=DIRECTION('',(-1.,0.,0.));
#8694=DIRECTION('center_axis',(0.,1.,0.));
#8695=DIRECTION('ref_axis',(0.,0.,1.));
#8696=DIRECTION('',(1.,0.,0.));
#8697=DIRECTION('center_axis',(-1.,0.,0.));
#8698=DIRECTION('ref_axis',(0.,6.12323399573677E-17,-1.));
#8699=DIRECTION('',(1.,0.,0.));
#8700=DIRECTION('center_axis',(1.,0.,0.));
#8701=DIRECTION('ref_axis',(0.,-6.12323399573677E-17,-1.));
#8702=DIRECTION('',(1.,0.,0.));
#8703=DIRECTION('',(1.,0.,0.));
#8704=DIRECTION('center_axis',(0.,1.,0.));
#8705=DIRECTION('ref_axis',(0.,0.,1.));
#8706=DIRECTION('center_axis',(0.,0.,-1.));
#8707=DIRECTION('ref_axis',(-1.,0.,0.));
#8708=DIRECTION('center_axis',(0.,-1.,0.));
#8709=DIRECTION('ref_axis',(1.,0.,0.));
#8710=DIRECTION('center_axis',(0.,-1.,0.));
#8711=DIRECTION('ref_axis',(1.,0.,0.));
#8712=DIRECTION('center_axis',(0.,-1.,0.));
#8713=DIRECTION('ref_axis',(1.,0.,0.));
#8714=DIRECTION('center_axis',(0.,0.,1.));
#8715=DIRECTION('ref_axis',(1.,0.,0.));
#8716=DIRECTION('center_axis',(-2.77555756156289E-16,1.,0.));
#8717=DIRECTION('ref_axis',(-1.,-2.77555756156289E-16,0.));
#8718=DIRECTION('center_axis',(0.,0.,1.));
#8719=DIRECTION('ref_axis',(1.,0.,0.));
#8720=DIRECTION('center_axis',(-1.,-5.9211894646675E-16,0.));
#8721=DIRECTION('ref_axis',(5.9211894646675E-16,-1.,0.));
#8722=DIRECTION('center_axis',(0.,0.,1.));
#8723=DIRECTION('ref_axis',(1.,0.,0.));
#8724=DIRECTION('center_axis',(1.,0.,0.));
#8725=DIRECTION('ref_axis',(0.,1.,0.));
#8726=DIRECTION('center_axis',(0.,-1.,0.));
#8727=DIRECTION('ref_axis',(0.,0.,-1.));
#8728=DIRECTION('center_axis',(0.,-1.,0.));
#8729=DIRECTION('ref_axis',(0.,0.,-1.));
#8730=DIRECTION('',(0.,0.,1.));
#8731=DIRECTION('',(1.,0.,0.));
#8732=DIRECTION('',(0.,0.,1.));
#8733=DIRECTION('',(1.,0.,0.));
#8734=DIRECTION('',(0.,0.,1.));
#8735=DIRECTION('',(1.,0.,0.));
#8736=DIRECTION('',(0.,0.,1.));
#8737=DIRECTION('',(1.,0.,0.));
#8738=DIRECTION('',(0.,0.,1.));
#8739=DIRECTION('',(1.,0.,0.));
#8740=DIRECTION('',(0.,0.,1.));
#8741=DIRECTION('',(1.,0.,0.));
#8742=DIRECTION('',(0.,0.,1.));
#8743=DIRECTION('',(1.,0.,0.));
#8744=DIRECTION('',(0.,0.,1.));
#8745=DIRECTION('',(1.,0.,0.));
#8746=DIRECTION('',(0.,0.,1.));
#8747=DIRECTION('',(1.,0.,0.));
#8748=DIRECTION('',(0.,0.,1.));
#8749=DIRECTION('',(1.,0.,0.));
#8750=CARTESIAN_POINT('',(0.,0.,0.));
#8751=CARTESIAN_POINT('',(0.,0.,0.));
#8752=CARTESIAN_POINT('Origin',(4.,0.,0.));
#8753=CARTESIAN_POINT('',(4.,-5.13675,6.29070444552017E-16));
#8754=CARTESIAN_POINT('Origin',(4.,0.,0.));
#8755=CARTESIAN_POINT('',(-4.,-5.13675,-6.29070444552017E-16));
#8756=CARTESIAN_POINT('',(4.,-5.13675,6.29070444552017E-16));
#8757=CARTESIAN_POINT('Origin',(-4.,0.,0.));
#8758=CARTESIAN_POINT('Origin',(4.,-10.,8.));
#8759=CARTESIAN_POINT('',(-4.,-10.,8.));
#8760=CARTESIAN_POINT('',(4.,-10.,8.));
#8761=CARTESIAN_POINT('',(2.,-10.,8.));
#8762=CARTESIAN_POINT('',(-4.,-10.,-7.859));
#8763=CARTESIAN_POINT('',(-4.,-10.,8.));
#8764=CARTESIAN_POINT('',(4.,-10.,-7.859));
#8765=CARTESIAN_POINT('',(4.,-10.,-7.859));
#8766=CARTESIAN_POINT('',(4.,-10.,8.));
#8767=CARTESIAN_POINT('Origin',(4.,10.,8.));
#8768=CARTESIAN_POINT('',(4.,10.,8.));
#8769=CARTESIAN_POINT('',(4.,-10.,8.));
#8770=CARTESIAN_POINT('',(4.,10.,-7.859));
#8771=CARTESIAN_POINT('',(4.,10.,-7.859));
#8772=CARTESIAN_POINT('',(4.,10.,8.));
#8773=CARTESIAN_POINT('Origin',(-4.,10.,8.));
#8774=CARTESIAN_POINT('',(-4.,10.,8.));
#8775=CARTESIAN_POINT('',(-2.,10.,8.));
#8776=CARTESIAN_POINT('',(-4.,10.,-7.859));
#8777=CARTESIAN_POINT('',(-4.,10.,-7.859));
#8778=CARTESIAN_POINT('',(-4.,10.,8.));
#8779=CARTESIAN_POINT('Origin',(-4.,-10.,8.));
#8780=CARTESIAN_POINT('',(-4.,-20.,8.));
#8781=CARTESIAN_POINT('',(-4.,-10.,-7.859));
#8782=CARTESIAN_POINT('Origin',(0.,0.,-7.859));
#8783=CARTESIAN_POINT('Origin',(29.7,21.9999999999999,-1.92966607280848));
#8784=CARTESIAN_POINT('',(30.,21.9999999999999,-7.22966607280848));
#8785=CARTESIAN_POINT('Origin',(30.,21.9999999999999,-1.92966607280848));
#8786=CARTESIAN_POINT('',(29.7,21.9999999999999,-6.92966607280848));
#8787=CARTESIAN_POINT('Origin',(29.7,21.9999999999999,-7.22966607280848));
#8788=CARTESIAN_POINT('',(29.7,16.9999999999999,-1.92966607280848));
#8789=CARTESIAN_POINT('Origin',(29.7,21.9999999999999,-1.92966607280848));
#8790=CARTESIAN_POINT('Origin',(29.7,21.9999999999999,-1.92966607280848));
#8791=CARTESIAN_POINT('Origin',(30.,0.,12.));
#8792=CARTESIAN_POINT('',(30.,-29.7,8.3));
#8793=CARTESIAN_POINT('',(30.,-29.7,15.7));
#8794=CARTESIAN_POINT('',(30.,-29.7,14.));
#8795=CARTESIAN_POINT('',(30.,-29.2999999999999,8.3));
#8796=CARTESIAN_POINT('',(30.,-15.,8.3));
#8797=CARTESIAN_POINT('',(30.,-28.6999999999999,7.7));
#8798=CARTESIAN_POINT('Origin',(30.,-29.2999999999999,7.7));
#8799=CARTESIAN_POINT('',(30.,-28.6999999999999,4.3));
#8800=CARTESIAN_POINT('',(30.,-28.6999999999999,8.));
#8801=CARTESIAN_POINT('',(30.,-28.2999999999999,4.3));
#8802=CARTESIAN_POINT('',(30.,-7.49999999999996,4.3));
#8803=CARTESIAN_POINT('',(30.,-27.6999999999999,3.7));
#8804=CARTESIAN_POINT('Origin',(30.,-28.2999999999999,3.7));
#8805=CARTESIAN_POINT('',(30.,-27.6999999999999,-7.55933214561695));
#8806=CARTESIAN_POINT('',(30.,-27.6999999999999,2.07033392719152));
#8807=CARTESIAN_POINT('',(30.,-16.2999999999999,-7.55933214561695));
#8808=CARTESIAN_POINT('',(30.,-7.99999999999996,-7.55933214561695));
#8809=CARTESIAN_POINT('',(30.,-16.2999999999999,4.3));
#8810=CARTESIAN_POINT('',(30.,-16.2999999999999,8.));
#8811=CARTESIAN_POINT('',(30.,-15.2999999999999,4.3));
#8812=CARTESIAN_POINT('',(30.,-7.49999999999996,4.3));
#8813=CARTESIAN_POINT('',(30.,-15.2999999999999,8.3));
#8814=CARTESIAN_POINT('',(30.,-15.2999999999999,10.));
#8815=CARTESIAN_POINT('',(30.,15.2999999999999,8.3));
#8816=CARTESIAN_POINT('',(30.,-15.,8.3));
#8817=CARTESIAN_POINT('',(30.,15.2999999999999,4.3));
#8818=CARTESIAN_POINT('',(30.,15.2999999999999,10.));
#8819=CARTESIAN_POINT('',(30.,16.2999999999999,4.3));
#8820=CARTESIAN_POINT('',(30.,7.49999999999996,4.3));
#8821=CARTESIAN_POINT('',(30.,16.2999999999999,-7.55933214561695));
#8822=CARTESIAN_POINT('',(30.,16.2999999999999,8.));
#8823=CARTESIAN_POINT('',(30.,27.6999999999999,-7.55933214561695));
#8824=CARTESIAN_POINT('',(30.,7.99999999999996,-7.55933214561695));
#8825=CARTESIAN_POINT('',(30.,27.6999999999999,3.7));
#8826=CARTESIAN_POINT('',(30.,27.6999999999999,2.07033392719152));
#8827=CARTESIAN_POINT('',(30.,28.2999999999999,4.3));
#8828=CARTESIAN_POINT('Origin',(30.,28.2999999999999,3.7));
#8829=CARTESIAN_POINT('',(30.,28.6999999999999,4.3));
#8830=CARTESIAN_POINT('',(30.,7.49999999999996,4.3));
#8831=CARTESIAN_POINT('',(30.,28.6999999999999,7.7));
#8832=CARTESIAN_POINT('',(30.,28.6999999999999,8.));
#8833=CARTESIAN_POINT('',(30.,29.2999999999999,8.3));
#8834=CARTESIAN_POINT('Origin',(30.,29.2999999999999,7.7));
#8835=CARTESIAN_POINT('',(30.,29.7,8.3));
#8836=CARTESIAN_POINT('',(30.,-15.,8.3));
#8837=CARTESIAN_POINT('',(30.,29.7,15.7));
#8838=CARTESIAN_POINT('',(30.,29.7,10.));
#8839=CARTESIAN_POINT('',(30.,15.,15.7));
#8840=CARTESIAN_POINT('',(30.,-21.9999999999999,3.37033392719152));
#8841=CARTESIAN_POINT('Origin',(30.,-21.9999999999999,-1.92966607280848));
#8842=CARTESIAN_POINT('Origin',(0.,21.9999999999999,-1.92966607280848));
#8843=CARTESIAN_POINT('',(-29.7,16.9999999999999,-1.92966607280848));
#8844=CARTESIAN_POINT('',(0.,16.9999999999999,-1.92966607280848));
#8845=CARTESIAN_POINT('',(-29.7,21.9999999999999,3.07033392719152));
#8846=CARTESIAN_POINT('Origin',(-29.7,21.9999999999999,-1.92966607280848));
#8847=CARTESIAN_POINT('Origin',(-29.7,21.9999999999999,-1.92966607280848));
#8848=CARTESIAN_POINT('Origin',(29.7,-21.9999999999999,-1.92966607280848));
#8849=CARTESIAN_POINT('',(29.7,-16.9999999999999,-1.92966607280848));
#8850=CARTESIAN_POINT('',(29.7,-21.9999999999999,3.07033392719152));
#8851=CARTESIAN_POINT('Origin',(29.7,-21.9999999999999,-1.92966607280848));
#8852=CARTESIAN_POINT('Origin',(29.7,-21.9999999999999,3.37033392719152));
#8853=CARTESIAN_POINT('Origin',(29.7,-21.9999999999999,-1.92966607280848));
#8854=CARTESIAN_POINT('Origin',(0.,-21.9999999999999,-1.92966607280848));
#8855=CARTESIAN_POINT('',(-29.7,-16.9999999999999,-1.92966607280848));
#8856=CARTESIAN_POINT('',(0.,-16.9999999999999,-1.92966607280848));
#8857=CARTESIAN_POINT('',(-29.7,-21.9999999999999,-6.92966607280848));
#8858=CARTESIAN_POINT('Origin',(-29.7,-21.9999999999999,-1.92966607280848));
#8859=CARTESIAN_POINT('Origin',(-29.7,-21.9999999999999,-1.92966607280848));
#8860=CARTESIAN_POINT('Origin',(-29.7,21.9999999999999,-1.92966607280848));
#8861=CARTESIAN_POINT('',(-30.,21.9999999999999,3.37033392719152));
#8862=CARTESIAN_POINT('Origin',(-30.,21.9999999999999,-1.92966607280848));
#8863=CARTESIAN_POINT('Origin',(-29.7,21.9999999999999,3.37033392719152));
#8864=CARTESIAN_POINT('Origin',(-30.,0.,12.));
#8865=CARTESIAN_POINT('',(-30.,-29.2999999999999,8.3));
#8866=CARTESIAN_POINT('',(-30.,-28.6999999999999,7.7));
#8867=CARTESIAN_POINT('Origin',(-30.,-29.2999999999999,7.7));
#8868=CARTESIAN_POINT('',(-30.,-29.7,8.3));
#8869=CARTESIAN_POINT('',(-30.,-15.,8.3));
#8870=CARTESIAN_POINT('',(-30.,-29.7,15.7));
#8871=CARTESIAN_POINT('',(-30.,-29.7,14.));
#8872=CARTESIAN_POINT('',(-30.,29.7,15.7));
#8873=CARTESIAN_POINT('',(-30.,15.,15.7));
#8874=CARTESIAN_POINT('',(-30.,29.7,8.3));
#8875=CARTESIAN_POINT('',(-30.,29.7,10.));
#8876=CARTESIAN_POINT('',(-30.,29.2999999999999,8.3));
#8877=CARTESIAN_POINT('',(-30.,-15.,8.3));
#8878=CARTESIAN_POINT('',(-30.,28.6999999999999,7.7));
#8879=CARTESIAN_POINT('Origin',(-30.,29.2999999999999,7.7));
#8880=CARTESIAN_POINT('',(-30.,28.6999999999999,4.3));
#8881=CARTESIAN_POINT('',(-30.,28.6999999999999,8.));
#8882=CARTESIAN_POINT('',(-30.,28.2999999999999,4.3));
#8883=CARTESIAN_POINT('',(-30.,7.49999999999996,4.3));
#8884=CARTESIAN_POINT('',(-30.,27.6999999999999,3.7));
#8885=CARTESIAN_POINT('Origin',(-30.,28.2999999999999,3.7));
#8886=CARTESIAN_POINT('',(-30.,27.6999999999999,-7.55933214561695));
#8887=CARTESIAN_POINT('',(-30.,27.6999999999999,2.07033392719152));
#8888=CARTESIAN_POINT('',(-30.,16.2999999999999,-7.55933214561695));
#8889=CARTESIAN_POINT('',(-30.,7.99999999999996,-7.55933214561695));
#8890=CARTESIAN_POINT('',(-30.,16.2999999999999,4.3));
#8891=CARTESIAN_POINT('',(-30.,16.2999999999999,8.));
#8892=CARTESIAN_POINT('',(-30.,15.2999999999999,4.3));
#8893=CARTESIAN_POINT('',(-30.,7.49999999999996,4.3));
#8894=CARTESIAN_POINT('',(-30.,15.2999999999999,8.3));
#8895=CARTESIAN_POINT('',(-30.,15.2999999999999,10.));
#8896=CARTESIAN_POINT('',(-30.,-15.2999999999999,8.3));
#8897=CARTESIAN_POINT('',(-30.,-15.,8.3));
#8898=CARTESIAN_POINT('',(-30.,-15.2999999999999,4.3));
#8899=CARTESIAN_POINT('',(-30.,-15.2999999999999,10.));
#8900=CARTESIAN_POINT('',(-30.,-16.2999999999999,4.3));
#8901=CARTESIAN_POINT('',(-30.,-7.49999999999996,4.3));
#8902=CARTESIAN_POINT('',(-30.,-16.2999999999999,-7.55933214561695));
#8903=CARTESIAN_POINT('',(-30.,-16.2999999999999,8.));
#8904=CARTESIAN_POINT('',(-30.,-27.6999999999999,-7.55933214561695));
#8905=CARTESIAN_POINT('',(-30.,-7.99999999999996,-7.55933214561695));
#8906=CARTESIAN_POINT('',(-30.,-27.6999999999999,3.7));
#8907=CARTESIAN_POINT('',(-30.,-27.6999999999999,2.07033392719152));
#8908=CARTESIAN_POINT('',(-30.,-28.2999999999999,4.3));
#8909=CARTESIAN_POINT('Origin',(-30.,-28.2999999999999,3.7));
#8910=CARTESIAN_POINT('',(-30.,-28.6999999999999,4.3));
#8911=CARTESIAN_POINT('',(-30.,-7.49999999999996,4.3));
#8912=CARTESIAN_POINT('',(-30.,-28.6999999999999,8.));
#8913=CARTESIAN_POINT('',(-30.,-21.9999999999999,-7.22966607280848));
#8914=CARTESIAN_POINT('Origin',(-30.,-21.9999999999999,-1.92966607280848));
#8915=CARTESIAN_POINT('Origin',(-29.7,-21.9999999999999,-1.92966607280848));
#8916=CARTESIAN_POINT('Origin',(-29.7,-21.9999999999999,-7.22966607280848));
#8917=CARTESIAN_POINT('Origin',(-14.1247849194883,-25.3746234146051,15.7));
#8918=CARTESIAN_POINT('',(-12.3247849194883,-25.3746234146051,16.));
#8919=CARTESIAN_POINT('Origin',(-14.1247849194883,-25.3746234146051,16.));
#8920=CARTESIAN_POINT('',(-12.6247849194883,-25.3746234146051,15.7));
#8921=CARTESIAN_POINT('Origin',(-12.3247849194883,-25.3746234146051,15.7));
#8922=CARTESIAN_POINT('Origin',(-14.1247849194883,-25.3746234146051,15.7));
#8923=CARTESIAN_POINT('Origin',(0.,30.,16.));
#8924=CARTESIAN_POINT('',(29.7,-29.7,16.));
#8925=CARTESIAN_POINT('',(-29.7,-29.7,16.));
#8926=CARTESIAN_POINT('',(0.,-29.7,16.));
#8927=CARTESIAN_POINT('',(29.7,29.7,16.));
#8928=CARTESIAN_POINT('',(29.7,15.,16.));
#8929=CARTESIAN_POINT('',(-29.7,29.7,16.));
#8930=CARTESIAN_POINT('',(0.,29.7,16.));
#8931=CARTESIAN_POINT('',(-29.7,15.,16.));
#8932=CARTESIAN_POINT('',(-21.3247849194883,-6.37462341460511,16.));
#8933=CARTESIAN_POINT('Origin',(-23.1247849194883,-6.37462341460511,16.));
#8934=CARTESIAN_POINT('',(15.9247849194883,-25.3746234146051,16.));
#8935=CARTESIAN_POINT('Origin',(14.1247849194883,-25.3746234146051,16.));
#8936=CARTESIAN_POINT('',(24.9247849194883,15.3746234146051,16.));
#8937=CARTESIAN_POINT('Origin',(23.1247849194883,15.3746234146051,16.));
#8938=CARTESIAN_POINT('',(-21.3247849194883,15.3746234146051,16.));
#8939=CARTESIAN_POINT('Origin',(-23.1247849194883,15.3746234146051,16.));
#8940=CARTESIAN_POINT('',(-21.3247849194883,6.37462341460511,16.));
#8941=CARTESIAN_POINT('Origin',(-23.1247849194883,6.37462341460511,16.));
#8942=CARTESIAN_POINT('',(15.9247849194883,25.3746234146051,16.));
#8943=CARTESIAN_POINT('Origin',(14.1247849194883,25.3746234146051,16.));
#8944=CARTESIAN_POINT('',(24.9247849194883,25.3746234146051,16.));
#8945=CARTESIAN_POINT('Origin',(23.1247849194883,25.3746234146051,16.));
#8946=CARTESIAN_POINT('',(-12.3247849194883,25.3746234146051,16.));
#8947=CARTESIAN_POINT('Origin',(-14.1247849194883,25.3746234146051,16.));
#8948=CARTESIAN_POINT('',(-21.3247849194883,25.3746234146051,16.));
#8949=CARTESIAN_POINT('Origin',(-23.1247849194883,25.3746234146051,16.));
#8950=CARTESIAN_POINT('',(24.9247849194883,-25.3746234146051,16.));
#8951=CARTESIAN_POINT('Origin',(23.1247849194883,-25.3746234146051,16.));
#8952=CARTESIAN_POINT('',(24.9247849194883,-15.3746234146051,16.));
#8953=CARTESIAN_POINT('Origin',(23.1247849194883,-15.3746234146051,16.));
#8954=CARTESIAN_POINT('',(-21.3247849194883,-25.3746234146051,16.));
#8955=CARTESIAN_POINT('Origin',(-23.1247849194883,-25.3746234146051,16.));
#8956=CARTESIAN_POINT('',(-21.3247849194883,-15.3746234146051,16.));
#8957=CARTESIAN_POINT('Origin',(-23.1247849194883,-15.3746234146051,16.));
#8958=CARTESIAN_POINT('',(24.9247849194883,6.37462341460511,16.));
#8959=CARTESIAN_POINT('Origin',(23.1247849194883,6.37462341460511,16.));
#8960=CARTESIAN_POINT('',(24.9247849194883,-6.37462341460511,16.));
#8961=CARTESIAN_POINT('Origin',(23.1247849194883,-6.37462341460511,16.));
#8962=CARTESIAN_POINT('Origin',(-14.1247849194883,-25.3746234146051,16.));
#8963=CARTESIAN_POINT('',(-12.6247849194883,-25.3746234146051,10.));
#8964=CARTESIAN_POINT('',(-12.6247849194883,-25.3746234146051,16.));
#8965=CARTESIAN_POINT('Origin',(-14.1247849194883,-25.3746234146051,10.));
#8966=CARTESIAN_POINT('Origin',(-23.1247849194883,-6.37462341460511,15.7));
#8967=CARTESIAN_POINT('',(-21.6247849194883,-6.37462341460511,15.7));
#8968=CARTESIAN_POINT('Origin',(-21.3247849194883,-6.37462341460511,15.7));
#8969=CARTESIAN_POINT('Origin',(-23.1247849194883,-6.37462341460511,15.7));
#8970=CARTESIAN_POINT('Origin',(-23.1247849194883,-6.37462341460511,16.));
#8971=CARTESIAN_POINT('',(-21.6247849194883,-6.37462341460511,10.));
#8972=CARTESIAN_POINT('',(-21.6247849194883,-6.37462341460511,16.));
#8973=CARTESIAN_POINT('Origin',(-23.1247849194883,-6.37462341460511,10.));
#8974=CARTESIAN_POINT('Origin',(23.1247849194883,-6.37462341460511,15.7));
#8975=CARTESIAN_POINT('',(24.6247849194883,-6.37462341460511,15.7));
#8976=CARTESIAN_POINT('Origin',(24.9247849194883,-6.37462341460511,15.7));
#8977=CARTESIAN_POINT('Origin',(23.1247849194883,-6.37462341460511,15.7));
#8978=CARTESIAN_POINT('Origin',(23.1247849194883,-6.37462341460511,16.));
#8979=CARTESIAN_POINT('',(24.6247849194883,-6.37462341460511,10.));
#8980=CARTESIAN_POINT('',(24.6247849194883,-6.37462341460511,16.));
#8981=CARTESIAN_POINT('Origin',(23.1247849194883,-6.37462341460511,10.));
#8982=CARTESIAN_POINT('Origin',(14.1247849194883,-25.3746234146051,15.7));
#8983=CARTESIAN_POINT('',(15.6247849194883,-25.3746234146051,15.7));
#8984=CARTESIAN_POINT('Origin',(15.9247849194883,-25.3746234146051,15.7));
#8985=CARTESIAN_POINT('Origin',(14.1247849194883,-25.3746234146051,15.7));
#8986=CARTESIAN_POINT('Origin',(14.1247849194883,-25.3746234146051,16.));
#8987=CARTESIAN_POINT('',(15.6247849194883,-25.3746234146051,10.));
#8988=CARTESIAN_POINT('',(15.6247849194883,-25.3746234146051,16.));
#8989=CARTESIAN_POINT('Origin',(14.1247849194883,-25.3746234146051,10.));
#8990=CARTESIAN_POINT('Origin',(23.1247849194883,6.37462341460511,15.7));
#8991=CARTESIAN_POINT('',(24.6247849194883,6.37462341460511,15.7));
#8992=CARTESIAN_POINT('Origin',(24.9247849194883,6.37462341460511,15.7));
#8993=CARTESIAN_POINT('Origin',(23.1247849194883,6.37462341460511,15.7));
#8994=CARTESIAN_POINT('Origin',(23.1247849194883,6.37462341460511,16.));
#8995=CARTESIAN_POINT('',(24.6247849194883,6.37462341460511,10.));
#8996=CARTESIAN_POINT('',(24.6247849194883,6.37462341460511,16.));
#8997=CARTESIAN_POINT('Origin',(23.1247849194883,6.37462341460511,10.));
#8998=CARTESIAN_POINT('Origin',(23.1247849194883,15.3746234146051,15.7));
#8999=CARTESIAN_POINT('',(24.6247849194883,15.3746234146051,15.7));
#9000=CARTESIAN_POINT('Origin',(24.9247849194883,15.3746234146051,15.7));
#9001=CARTESIAN_POINT('Origin',(23.1247849194883,15.3746234146051,15.7));
#9002=CARTESIAN_POINT('Origin',(23.1247849194883,15.3746234146051,16.));
#9003=CARTESIAN_POINT('',(24.6247849194883,15.3746234146051,10.));
#9004=CARTESIAN_POINT('',(24.6247849194883,15.3746234146051,16.));
#9005=CARTESIAN_POINT('Origin',(23.1247849194883,15.3746234146051,10.));
#9006=CARTESIAN_POINT('Origin',(-23.1247849194883,-15.3746234146051,15.7));
#9007=CARTESIAN_POINT('',(-21.6247849194883,-15.3746234146051,15.7));
#9008=CARTESIAN_POINT('Origin',(-21.3247849194883,-15.3746234146051,15.7));
#9009=CARTESIAN_POINT('Origin',(-23.1247849194883,-15.3746234146051,15.7));
#9010=CARTESIAN_POINT('Origin',(-23.1247849194883,-15.3746234146051,16.));
#9011=CARTESIAN_POINT('',(-21.6247849194883,-15.3746234146051,10.));
#9012=CARTESIAN_POINT('',(-21.6247849194883,-15.3746234146051,16.));
#9013=CARTESIAN_POINT('Origin',(-23.1247849194883,-15.3746234146051,10.));
#9014=CARTESIAN_POINT('Origin',(-23.1247849194883,15.3746234146051,15.7));
#9015=CARTESIAN_POINT('',(-21.6247849194883,15.3746234146051,15.7));
#9016=CARTESIAN_POINT('Origin',(-21.3247849194883,15.3746234146051,15.7));
#9017=CARTESIAN_POINT('',(-23.1247849194883,13.8746234146051,15.7));
#9018=CARTESIAN_POINT('Origin',(-23.1247849194883,15.3746234146051,15.7));
#9019=CARTESIAN_POINT('Origin',(-23.1247849194883,15.3746234146051,15.7));
#9020=CARTESIAN_POINT('Origin',(-23.1247849194883,15.3746234146051,16.));
#9021=CARTESIAN_POINT('',(-23.1247849194883,13.8746234146051,10.));
#9022=CARTESIAN_POINT('',(-23.1247849194883,13.8746234146051,16.));
#9023=CARTESIAN_POINT('Origin',(-23.1247849194883,15.3746234146051,10.));
#9024=CARTESIAN_POINT('Origin',(-23.1247849194883,-25.3746234146051,15.7));
#9025=CARTESIAN_POINT('',(-21.6247849194883,-25.3746234146051,15.7));
#9026=CARTESIAN_POINT('Origin',(-21.3247849194883,-25.3746234146051,15.7));
#9027=CARTESIAN_POINT('Origin',(-23.1247849194883,-25.3746234146051,15.7));
#9028=CARTESIAN_POINT('Origin',(-23.1247849194883,-25.3746234146051,16.));
#9029=CARTESIAN_POINT('',(-21.6247849194883,-25.3746234146051,10.));
#9030=CARTESIAN_POINT('',(-21.6247849194883,-25.3746234146051,16.));
#9031=CARTESIAN_POINT('Origin',(-23.1247849194883,-25.3746234146051,10.));
#9032=CARTESIAN_POINT('Origin',(-23.1247849194883,6.37462341460511,15.7));
#9033=CARTESIAN_POINT('',(-21.6247849194883,6.37462341460511,15.7));
#9034=CARTESIAN_POINT('Origin',(-21.3247849194883,6.37462341460511,15.7));
#9035=CARTESIAN_POINT('',(-23.1247849194883,4.87462341460511,15.7));
#9036=CARTESIAN_POINT('Origin',(-23.1247849194883,6.37462341460511,15.7));
#9037=CARTESIAN_POINT('Origin',(-23.1247849194883,6.37462341460511,15.7));
#9038=CARTESIAN_POINT('Origin',(-23.1247849194883,6.37462341460511,16.));
#9039=CARTESIAN_POINT('',(-23.1247849194883,4.87462341460511,10.));
#9040=CARTESIAN_POINT('',(-23.1247849194883,4.87462341460511,16.));
#9041=CARTESIAN_POINT('Origin',(-23.1247849194883,6.37462341460511,10.));
#9042=CARTESIAN_POINT('Origin',(23.1247849194883,-15.3746234146051,15.7));
#9043=CARTESIAN_POINT('',(24.6247849194883,-15.3746234146051,15.7));
#9044=CARTESIAN_POINT('Origin',(24.9247849194883,-15.3746234146051,15.7));
#9045=CARTESIAN_POINT('Origin',(23.1247849194883,-15.3746234146051,15.7));
#9046=CARTESIAN_POINT('Origin',(23.1247849194883,-15.3746234146051,16.));
#9047=CARTESIAN_POINT('',(24.6247849194883,-15.3746234146051,10.));
#9048=CARTESIAN_POINT('',(24.6247849194883,-15.3746234146051,16.));
#9049=CARTESIAN_POINT('Origin',(23.1247849194883,-15.3746234146051,10.));
#9050=CARTESIAN_POINT('Origin',(14.1247849194883,25.3746234146051,15.7));
#9051=CARTESIAN_POINT('',(15.6247849194883,25.3746234146051,15.7));
#9052=CARTESIAN_POINT('Origin',(15.9247849194883,25.3746234146051,15.7));
#9053=CARTESIAN_POINT('Origin',(14.1247849194883,25.3746234146051,15.7));
#9054=CARTESIAN_POINT('Origin',(14.1247849194883,25.3746234146051,16.));
#9055=CARTESIAN_POINT('',(15.6247849194883,25.3746234146051,10.));
#9056=CARTESIAN_POINT('',(15.6247849194883,25.3746234146051,16.));
#9057=CARTESIAN_POINT('Origin',(14.1247849194883,25.3746234146051,10.));
#9058=CARTESIAN_POINT('Origin',(23.1247849194883,-25.3746234146051,15.7));
#9059=CARTESIAN_POINT('',(24.6247849194883,-25.3746234146051,15.7));
#9060=CARTESIAN_POINT('Origin',(24.9247849194883,-25.3746234146051,15.7));
#9061=CARTESIAN_POINT('Origin',(23.1247849194883,-25.3746234146051,15.7));
#9062=CARTESIAN_POINT('Origin',(23.1247849194883,-25.3746234146051,16.));
#9063=CARTESIAN_POINT('',(24.6247849194883,-25.3746234146051,10.));
#9064=CARTESIAN_POINT('',(24.6247849194883,-25.3746234146051,16.));
#9065=CARTESIAN_POINT('Origin',(23.1247849194883,-25.3746234146051,10.));
#9066=CARTESIAN_POINT('Origin',(23.1247849194883,25.3746234146051,15.7));
#9067=CARTESIAN_POINT('',(24.6247849194883,25.3746234146051,15.7));
#9068=CARTESIAN_POINT('Origin',(24.9247849194883,25.3746234146051,15.7));
#9069=CARTESIAN_POINT('Origin',(23.1247849194883,25.3746234146051,15.7));
#9070=CARTESIAN_POINT('Origin',(23.1247849194883,25.3746234146051,16.));
#9071=CARTESIAN_POINT('',(24.6247849194883,25.3746234146051,10.));
#9072=CARTESIAN_POINT('',(24.6247849194883,25.3746234146051,16.));
#9073=CARTESIAN_POINT('Origin',(23.1247849194883,25.3746234146051,10.));
#9074=CARTESIAN_POINT('Origin',(-23.1247849194883,25.3746234146051,15.7));
#9075=CARTESIAN_POINT('',(-21.6247849194883,25.3746234146051,15.7));
#9076=CARTESIAN_POINT('Origin',(-21.3247849194883,25.3746234146051,15.7));
#9077=CARTESIAN_POINT('Origin',(-23.1247849194883,25.3746234146051,15.7));
#9078=CARTESIAN_POINT('Origin',(-23.1247849194883,25.3746234146051,16.));
#9079=CARTESIAN_POINT('',(-21.6247849194883,25.3746234146051,10.));
#9080=CARTESIAN_POINT('',(-21.6247849194883,25.3746234146051,16.));
#9081=CARTESIAN_POINT('Origin',(-23.1247849194883,25.3746234146051,10.));
#9082=CARTESIAN_POINT('Origin',(-14.1247849194883,25.3746234146051,15.7));
#9083=CARTESIAN_POINT('',(-12.6247849194883,25.3746234146051,15.7));
#9084=CARTESIAN_POINT('Origin',(-12.3247849194883,25.3746234146051,15.7));
#9085=CARTESIAN_POINT('Origin',(-14.1247849194883,25.3746234146051,15.7));
#9086=CARTESIAN_POINT('Origin',(-14.1247849194883,25.3746234146051,16.));
#9087=CARTESIAN_POINT('',(-12.6247849194883,25.3746234146051,10.));
#9088=CARTESIAN_POINT('',(-12.6247849194883,25.3746234146051,16.));
#9089=CARTESIAN_POINT('Origin',(-14.1247849194883,25.3746234146051,10.));
#9090=CARTESIAN_POINT('Origin',(29.7,-15.,8.3));
#9091=CARTESIAN_POINT('',(29.7,-14.9999999999999,8.));
#9092=CARTESIAN_POINT('Origin',(29.7,-15.2999999999999,8.3));
#9093=CARTESIAN_POINT('',(29.7,14.9999999999999,8.));
#9094=CARTESIAN_POINT('',(29.7,-15.,8.));
#9095=CARTESIAN_POINT('Origin',(29.7,15.2999999999999,8.3));
#9096=CARTESIAN_POINT('Origin',(-29.7,-15.,8.3));
#9097=CARTESIAN_POINT('',(-29.7,14.9999999999999,8.));
#9098=CARTESIAN_POINT('Origin',(-29.7,15.2999999999999,8.3));
#9099=CARTESIAN_POINT('',(-29.7,-14.9999999999999,8.));
#9100=CARTESIAN_POINT('',(-29.7,-15.,8.));
#9101=CARTESIAN_POINT('Origin',(-29.7,-15.2999999999999,8.3));
#9102=CARTESIAN_POINT('Origin',(-29.7,15.2999999999999,10.));
#9103=CARTESIAN_POINT('',(-29.7,14.9999999999999,4.));
#9104=CARTESIAN_POINT('Origin',(-29.7,15.2999999999999,4.3));
#9105=CARTESIAN_POINT('',(-29.7,14.9999999999999,10.));
#9106=CARTESIAN_POINT('Origin',(29.7,-15.2999999999999,10.));
#9107=CARTESIAN_POINT('',(29.7,-14.9999999999999,4.));
#9108=CARTESIAN_POINT('Origin',(29.7,-15.2999999999999,4.3));
#9109=CARTESIAN_POINT('',(29.7,-14.9999999999999,10.));
#9110=CARTESIAN_POINT('Origin',(-29.7,7.49999999999996,4.3));
#9111=CARTESIAN_POINT('',(-29.7,15.9999999999999,4.));
#9112=CARTESIAN_POINT('Origin',(-29.7,16.2999999999999,4.3));
#9113=CARTESIAN_POINT('',(-29.7,7.49999999999996,4.));
#9114=CARTESIAN_POINT('Origin',(29.7,-7.49999999999996,4.3));
#9115=CARTESIAN_POINT('',(29.7,-15.9999999999999,4.));
#9116=CARTESIAN_POINT('Origin',(29.7,-16.2999999999999,4.3));
#9117=CARTESIAN_POINT('',(29.7,-7.49999999999996,4.));
#9118=CARTESIAN_POINT('Origin',(-29.7,-7.49999999999996,4.3));
#9119=CARTESIAN_POINT('',(-29.7,-14.9999999999999,4.));
#9120=CARTESIAN_POINT('',(-29.7,-15.9999999999999,4.));
#9121=CARTESIAN_POINT('',(-29.7,-7.49999999999996,4.));
#9122=CARTESIAN_POINT('Origin',(-29.7,-16.2999999999999,4.3));
#9123=CARTESIAN_POINT('Origin',(-29.7,-15.2999999999999,4.3));
#9124=CARTESIAN_POINT('Origin',(-29.7,16.2999999999999,8.));
#9125=CARTESIAN_POINT('',(-29.7,15.9999999999999,-7.85933214561696));
#9126=CARTESIAN_POINT('Origin',(-29.7,16.2999999999999,-7.55933214561695));
#9127=CARTESIAN_POINT('',(-29.7,15.9999999999999,8.));
#9128=CARTESIAN_POINT('Origin',(29.7,27.6999999999999,-7.55933214561695));
#9129=CARTESIAN_POINT('',(29.7,27.6999999999999,-7.85933214561696));
#9130=CARTESIAN_POINT('Origin',(29.7,27.6999999999999,-7.55933214561695));
#9131=CARTESIAN_POINT('',(29.7,27.9999999999999,-7.55933214561695));
#9132=CARTESIAN_POINT('Origin',(29.7,27.6999999999999,-7.55933214561695));
#9133=CARTESIAN_POINT('Origin',(29.7,27.6999999999999,-7.55933214561695));
#9134=CARTESIAN_POINT('Origin',(-29.7,27.6999999999999,-7.55933214561695));
#9135=CARTESIAN_POINT('',(-29.7,27.9999999999999,-7.55933214561695));
#9136=CARTESIAN_POINT('Origin',(-29.7,27.6999999999999,-7.55933214561695));
#9137=CARTESIAN_POINT('',(-29.7,27.6999999999999,-7.85933214561696));
#9138=CARTESIAN_POINT('Origin',(-29.7,27.6999999999999,-7.55933214561695));
#9139=CARTESIAN_POINT('Origin',(-29.7,27.6999999999999,-7.55933214561695));
#9140=CARTESIAN_POINT('Origin',(0.,27.6999999999999,-7.55933214561695));
#9141=CARTESIAN_POINT('',(0.,27.6999999999999,-7.85933214561696));
#9142=CARTESIAN_POINT('',(0.,27.9999999999999,-7.55933214561695));
#9143=CARTESIAN_POINT('Origin',(-29.7,7.99999999999996,-7.55933214561695));
#9144=CARTESIAN_POINT('',(-29.7,7.99999999999996,-7.85933214561696));
#9145=CARTESIAN_POINT('Origin',(29.7,-27.6999999999999,-7.55933214561695));
#9146=CARTESIAN_POINT('',(29.7,-27.6999999999999,-7.85933214561696));
#9147=CARTESIAN_POINT('',(29.7,-27.9999999999999,-7.55933214561695));
#9148=CARTESIAN_POINT('Origin',(29.7,-27.6999999999999,-7.55933214561695));
#9149=CARTESIAN_POINT('Origin',(29.7,-27.6999999999999,-7.55933214561695));
#9150=CARTESIAN_POINT('Origin',(29.7,-27.6999999999999,-7.55933214561695));
#9151=CARTESIAN_POINT('Origin',(29.7,-7.99999999999996,-7.55933214561695));
#9152=CARTESIAN_POINT('',(29.7,-15.9999999999999,-7.85933214561696));
#9153=CARTESIAN_POINT('',(29.7,-7.99999999999996,-7.85933214561696));
#9154=CARTESIAN_POINT('Origin',(29.7,-16.2999999999999,-7.55933214561695));
#9155=CARTESIAN_POINT('Origin',(29.7,28.2999999999999,3.7));
#9156=CARTESIAN_POINT('',(29.7,28.2999999999999,4.));
#9157=CARTESIAN_POINT('',(29.7,27.9999999999999,3.7));
#9158=CARTESIAN_POINT('Origin',(29.7,28.2999999999999,3.7));
#9159=CARTESIAN_POINT('Origin',(29.7,28.2999999999999,4.3));
#9160=CARTESIAN_POINT('Origin',(29.7,27.6999999999999,3.7));
#9161=CARTESIAN_POINT('Origin',(-29.7,-27.6999999999999,-7.55933214561695));
#9162=CARTESIAN_POINT('',(-29.7,-27.9999999999999,-7.55933214561695));
#9163=CARTESIAN_POINT('Origin',(-29.7,-27.6999999999999,-7.55933214561695));
#9164=CARTESIAN_POINT('',(-29.7,-27.6999999999999,-7.85933214561696));
#9165=CARTESIAN_POINT('Origin',(-29.7,-27.6999999999999,-7.55933214561695));
#9166=CARTESIAN_POINT('Origin',(-29.7,-27.6999999999999,-7.55933214561695));
#9167=CARTESIAN_POINT('Origin',(-29.7,-7.99999999999996,-7.55933214561695));
#9168=CARTESIAN_POINT('',(-29.7,-15.9999999999999,-7.85933214561696));
#9169=CARTESIAN_POINT('',(-29.7,-7.99999999999996,-7.85933214561696));
#9170=CARTESIAN_POINT('Origin',(-29.7,-16.2999999999999,-7.55933214561695));
#9171=CARTESIAN_POINT('Origin',(0.,-27.6999999999999,-7.55933214561695));
#9172=CARTESIAN_POINT('',(0.,-27.9999999999999,-7.55933214561695));
#9173=CARTESIAN_POINT('',(0.,-27.6999999999999,-7.85933214561696));
#9174=CARTESIAN_POINT('Origin',(-29.7,28.2999999999999,3.7));
#9175=CARTESIAN_POINT('',(-29.7,27.9999999999999,3.7));
#9176=CARTESIAN_POINT('',(-29.7,28.2999999999999,4.));
#9177=CARTESIAN_POINT('Origin',(-29.7,28.2999999999999,3.7));
#9178=CARTESIAN_POINT('Origin',(-29.7,27.6999999999999,3.7));
#9179=CARTESIAN_POINT('Origin',(-29.7,28.2999999999999,4.3));
#9180=CARTESIAN_POINT('Origin',(-29.7,27.6999999999999,2.07033392719152));
#9181=CARTESIAN_POINT('',(-29.7,27.9999999999999,2.07033392719152));
#9182=CARTESIAN_POINT('Origin',(29.7,-28.2999999999999,3.7));
#9183=CARTESIAN_POINT('',(29.7,-28.2999999999999,4.));
#9184=CARTESIAN_POINT('Origin',(29.7,-28.2999999999999,4.3));
#9185=CARTESIAN_POINT('',(29.7,-27.9999999999999,3.7));
#9186=CARTESIAN_POINT('Origin',(29.7,-28.2999999999999,3.7));
#9187=CARTESIAN_POINT('Origin',(29.7,-27.6999999999999,3.7));
#9188=CARTESIAN_POINT('Origin',(29.7,28.6999999999999,4.3));
#9189=CARTESIAN_POINT('',(29.7,28.6999999999999,4.));
#9190=CARTESIAN_POINT('Origin',(29.7,28.6999999999999,4.3));
#9191=CARTESIAN_POINT('',(29.7,28.9999999999999,4.3));
#9192=CARTESIAN_POINT('Origin',(29.7,28.6999999999999,4.3));
#9193=CARTESIAN_POINT('Origin',(29.7,28.6999999999999,4.3));
#9194=CARTESIAN_POINT('Origin',(-29.7,-28.2999999999999,3.7));
#9195=CARTESIAN_POINT('',(-29.7,-28.2999999999999,4.));
#9196=CARTESIAN_POINT('',(-29.7,-27.9999999999999,3.7));
#9197=CARTESIAN_POINT('Origin',(-29.7,-28.2999999999999,3.7));
#9198=CARTESIAN_POINT('Origin',(-29.7,-28.2999999999999,4.3));
#9199=CARTESIAN_POINT('Origin',(-29.7,-27.6999999999999,3.7));
#9200=CARTESIAN_POINT('Origin',(-29.7,28.6999999999999,4.3));
#9201=CARTESIAN_POINT('',(-29.7,28.9999999999999,4.3));
#9202=CARTESIAN_POINT('Origin',(-29.7,28.6999999999999,4.3));
#9203=CARTESIAN_POINT('',(-29.7,28.6999999999999,4.));
#9204=CARTESIAN_POINT('Origin',(-29.7,28.6999999999999,4.3));
#9205=CARTESIAN_POINT('Origin',(-29.7,28.6999999999999,4.3));
#9206=CARTESIAN_POINT('Origin',(0.,28.6999999999999,4.3));
#9207=CARTESIAN_POINT('',(0.,28.6999999999999,4.));
#9208=CARTESIAN_POINT('',(0.,28.9999999999999,4.3));
#9209=CARTESIAN_POINT('Origin',(-29.7,7.49999999999996,4.3));
#9210=CARTESIAN_POINT('',(-29.7,7.49999999999996,4.));
#9211=CARTESIAN_POINT('Origin',(29.7,-28.6999999999999,4.3));
#9212=CARTESIAN_POINT('',(29.7,-28.9999999999999,4.3));
#9213=CARTESIAN_POINT('Origin',(29.7,-28.6999999999999,4.3));
#9214=CARTESIAN_POINT('',(29.7,-28.6999999999999,4.));
#9215=CARTESIAN_POINT('Origin',(29.7,-28.6999999999999,4.3));
#9216=CARTESIAN_POINT('Origin',(29.7,-28.6999999999999,4.3));
#9217=CARTESIAN_POINT('Origin',(29.7,29.2999999999999,7.7));
#9218=CARTESIAN_POINT('',(29.7,29.2999999999999,8.));
#9219=CARTESIAN_POINT('',(29.7,28.9999999999999,7.7));
#9220=CARTESIAN_POINT('Origin',(29.7,29.2999999999999,7.7));
#9221=CARTESIAN_POINT('Origin',(29.7,29.2999999999999,8.3));
#9222=CARTESIAN_POINT('Origin',(29.7,28.6999999999999,7.7));
#9223=CARTESIAN_POINT('Origin',(-29.7,-28.6999999999999,4.3));
#9224=CARTESIAN_POINT('',(-29.7,-28.6999999999999,4.));
#9225=CARTESIAN_POINT('Origin',(-29.7,-28.6999999999999,4.3));
#9226=CARTESIAN_POINT('',(-29.7,-28.9999999999999,4.3));
#9227=CARTESIAN_POINT('Origin',(-29.7,-28.6999999999999,4.3));
#9228=CARTESIAN_POINT('Origin',(-29.7,-28.6999999999999,4.3));
#9229=CARTESIAN_POINT('Origin',(0.,-28.6999999999999,4.3));
#9230=CARTESIAN_POINT('',(0.,-28.9999999999999,4.3));
#9231=CARTESIAN_POINT('',(0.,-28.6999999999999,4.));
#9232=CARTESIAN_POINT('Origin',(-29.7,29.2999999999999,7.7));
#9233=CARTESIAN_POINT('',(-29.7,28.9999999999999,7.7));
#9234=CARTESIAN_POINT('',(-29.7,29.2999999999999,8.));
#9235=CARTESIAN_POINT('Origin',(-29.7,29.2999999999999,7.7));
#9236=CARTESIAN_POINT('Origin',(-29.7,28.6999999999999,7.7));
#9237=CARTESIAN_POINT('Origin',(-29.7,29.2999999999999,8.3));
#9238=CARTESIAN_POINT('Origin',(-29.7,28.6999999999999,8.));
#9239=CARTESIAN_POINT('',(-29.7,28.9999999999999,8.));
#9240=CARTESIAN_POINT('Origin',(29.7,-29.2999999999999,7.7));
#9241=CARTESIAN_POINT('',(29.7,-28.9999999999999,7.7));
#9242=CARTESIAN_POINT('',(29.7,-29.2999999999999,8.));
#9243=CARTESIAN_POINT('Origin',(29.7,-29.2999999999999,7.7));
#9244=CARTESIAN_POINT('Origin',(29.7,-28.6999999999999,7.7));
#9245=CARTESIAN_POINT('Origin',(29.7,-29.2999999999999,8.3));
#9246=CARTESIAN_POINT('Origin',(29.7,-28.6999999999999,8.));
#9247=CARTESIAN_POINT('',(29.7,-28.9999999999999,8.));
#9248=CARTESIAN_POINT('Origin',(29.7,29.7,8.3));
#9249=CARTESIAN_POINT('',(29.7,29.7,8.));
#9250=CARTESIAN_POINT('Origin',(29.7,29.7,8.3));
#9251=CARTESIAN_POINT('',(29.7,30.,8.3));
#9252=CARTESIAN_POINT('Origin',(29.7,29.7,8.3));
#9253=CARTESIAN_POINT('Origin',(29.7,29.7,8.3));
#9254=CARTESIAN_POINT('Origin',(-29.7,-29.2999999999999,7.7));
#9255=CARTESIAN_POINT('',(-29.7,-29.2999999999999,8.));
#9256=CARTESIAN_POINT('',(-29.7,-28.9999999999999,7.7));
#9257=CARTESIAN_POINT('Origin',(-29.7,-29.2999999999999,7.7));
#9258=CARTESIAN_POINT('Origin',(-29.7,-29.2999999999999,8.3));
#9259=CARTESIAN_POINT('Origin',(-29.7,-28.6999999999999,7.7));
#9260=CARTESIAN_POINT('Origin',(-29.7,29.7,8.3));
#9261=CARTESIAN_POINT('',(-29.7,30.,8.3));
#9262=CARTESIAN_POINT('Origin',(-29.7,29.7,8.3));
#9263=CARTESIAN_POINT('',(-29.7,29.7,8.));
#9264=CARTESIAN_POINT('Origin',(-29.7,29.7,8.3));
#9265=CARTESIAN_POINT('Origin',(-29.7,29.7,8.3));
#9266=CARTESIAN_POINT('Origin',(0.,29.7,8.3));
#9267=CARTESIAN_POINT('',(0.,29.7,8.));
#9268=CARTESIAN_POINT('',(0.,30.,8.3));
#9269=CARTESIAN_POINT('Origin',(-29.7,-15.,8.3));
#9270=CARTESIAN_POINT('',(-29.7,-15.,8.));
#9271=CARTESIAN_POINT('Origin',(29.7,-29.7,8.3));
#9272=CARTESIAN_POINT('',(29.7,-30.,8.3));
#9273=CARTESIAN_POINT('Origin',(29.7,-29.7,8.3));
#9274=CARTESIAN_POINT('',(29.7,-29.7,8.));
#9275=CARTESIAN_POINT('Origin',(29.7,-29.7,8.3));
#9276=CARTESIAN_POINT('Origin',(29.7,-29.7,8.3));
#9277=CARTESIAN_POINT('Origin',(29.7,29.7,15.7));
#9278=CARTESIAN_POINT('',(29.7,30.,15.7));
#9279=CARTESIAN_POINT('Origin',(29.7,29.7,15.7));
#9280=CARTESIAN_POINT('Origin',(29.7,29.7,15.7));
#9281=CARTESIAN_POINT('Origin',(29.7,29.7,15.7));
#9282=CARTESIAN_POINT('Origin',(-29.7,-29.7,8.3));
#9283=CARTESIAN_POINT('',(-29.7,-29.7,8.));
#9284=CARTESIAN_POINT('Origin',(-29.7,-29.7,8.3));
#9285=CARTESIAN_POINT('',(-29.7,-30.,8.3));
#9286=CARTESIAN_POINT('Origin',(-29.7,-29.7,8.3));
#9287=CARTESIAN_POINT('Origin',(-29.7,-29.7,8.3));
#9288=CARTESIAN_POINT('Origin',(0.,-29.7,8.3));
#9289=CARTESIAN_POINT('',(0.,-30.,8.3));
#9290=CARTESIAN_POINT('',(0.,-29.7,8.));
#9291=CARTESIAN_POINT('Origin',(-29.7,29.7,15.7));
#9292=CARTESIAN_POINT('Origin',(-29.7,29.7,15.7));
#9293=CARTESIAN_POINT('',(-29.7,30.,15.7));
#9294=CARTESIAN_POINT('Origin',(-29.7,29.7,15.7));
#9295=CARTESIAN_POINT('Origin',(-29.7,29.7,15.7));
#9296=CARTESIAN_POINT('Origin',(0.,29.7,15.7));
#9297=CARTESIAN_POINT('',(0.,30.,15.7));
#9298=CARTESIAN_POINT('Origin',(-29.7,29.7,10.));
#9299=CARTESIAN_POINT('',(-29.7,30.,10.));
#9300=CARTESIAN_POINT('Origin',(29.7,-29.7,15.7));
#9301=CARTESIAN_POINT('Origin',(29.7,-29.7,15.7));
#9302=CARTESIAN_POINT('',(29.7,-30.,15.7));
#9303=CARTESIAN_POINT('Origin',(29.7,-29.7,15.7));
#9304=CARTESIAN_POINT('Origin',(29.7,-29.7,15.7));
#9305=CARTESIAN_POINT('Origin',(-29.7,-29.7,15.7));
#9306=CARTESIAN_POINT('',(-29.7,-30.,15.7));
#9307=CARTESIAN_POINT('Origin',(-29.7,-29.7,15.7));
#9308=CARTESIAN_POINT('Origin',(-29.7,-29.7,15.7));
#9309=CARTESIAN_POINT('Origin',(-29.7,-29.7,15.7));
#9310=CARTESIAN_POINT('Origin',(0.,-29.7,15.7));
#9311=CARTESIAN_POINT('',(0.,-30.,15.7));
#9312=CARTESIAN_POINT('Origin',(-29.7,15.,15.7));
#9313=CARTESIAN_POINT('Origin',(-29.7,-29.7,14.));
#9314=CARTESIAN_POINT('',(-29.7,-30.,14.));
#9315=CARTESIAN_POINT('Origin',(29.7,-29.7,14.));
#9316=CARTESIAN_POINT('',(29.7,-30.,14.));
#9317=CARTESIAN_POINT('Origin',(29.7,15.,15.7));
#9318=CARTESIAN_POINT('Origin',(-29.7,-15.,8.3));
#9319=CARTESIAN_POINT('',(-29.7,-15.,8.));
#9320=CARTESIAN_POINT('Origin',(29.7,29.7,10.));
#9321=CARTESIAN_POINT('',(29.7,30.,10.));
#9322=CARTESIAN_POINT('Origin',(29.7,-15.,8.3));
#9323=CARTESIAN_POINT('',(29.7,-15.,8.));
#9324=CARTESIAN_POINT('Origin',(-29.7,-28.6999999999999,8.));
#9325=CARTESIAN_POINT('',(-29.7,-28.9999999999999,8.));
#9326=CARTESIAN_POINT('Origin',(0.,-29.2999999999999,7.7));
#9327=CARTESIAN_POINT('',(0.,-29.2999999999999,8.));
#9328=CARTESIAN_POINT('',(0.,-28.9999999999999,7.7));
#9329=CARTESIAN_POINT('Origin',(29.7,-15.,8.3));
#9330=CARTESIAN_POINT('',(29.7,-15.,8.));
#9331=CARTESIAN_POINT('Origin',(0.,29.2999999999999,7.7));
#9332=CARTESIAN_POINT('',(0.,29.2999999999999,8.));
#9333=CARTESIAN_POINT('',(0.,28.9999999999999,7.7));
#9334=CARTESIAN_POINT('Origin',(-29.7,-7.49999999999996,4.3));
#9335=CARTESIAN_POINT('',(-29.7,-7.49999999999996,4.));
#9336=CARTESIAN_POINT('Origin',(29.7,28.6999999999999,8.));
#9337=CARTESIAN_POINT('',(29.7,28.9999999999999,8.));
#9338=CARTESIAN_POINT('Origin',(29.7,-7.49999999999996,4.3));
#9339=CARTESIAN_POINT('',(29.7,-7.49999999999996,4.));
#9340=CARTESIAN_POINT('Origin',(-29.7,-27.6999999999999,2.07033392719152));
#9341=CARTESIAN_POINT('',(-29.7,-27.9999999999999,2.07033392719152));
#9342=CARTESIAN_POINT('Origin',(0.,-28.2999999999999,3.7));
#9343=CARTESIAN_POINT('',(0.,-28.2999999999999,4.));
#9344=CARTESIAN_POINT('',(0.,-27.9999999999999,3.7));
#9345=CARTESIAN_POINT('Origin',(29.7,7.49999999999996,4.3));
#9346=CARTESIAN_POINT('',(29.7,7.49999999999996,4.));
#9347=CARTESIAN_POINT('Origin',(29.7,-27.6999999999999,2.07033392719152));
#9348=CARTESIAN_POINT('',(29.7,-27.9999999999999,2.07033392719152));
#9349=CARTESIAN_POINT('Origin',(0.,28.2999999999999,3.7));
#9350=CARTESIAN_POINT('',(0.,28.2999999999999,4.));
#9351=CARTESIAN_POINT('',(0.,27.9999999999999,3.7));
#9352=CARTESIAN_POINT('Origin',(29.7,27.6999999999999,2.07033392719152));
#9353=CARTESIAN_POINT('',(29.7,27.9999999999999,2.07033392719152));
#9354=CARTESIAN_POINT('Origin',(-29.7,-16.2999999999999,8.));
#9355=CARTESIAN_POINT('',(-29.7,-15.9999999999999,8.));
#9356=CARTESIAN_POINT('Origin',(29.7,7.99999999999996,-7.55933214561695));
#9357=CARTESIAN_POINT('',(29.7,15.9999999999999,-7.85933214561696));
#9358=CARTESIAN_POINT('',(29.7,7.99999999999996,-7.85933214561696));
#9359=CARTESIAN_POINT('Origin',(29.7,16.2999999999999,-7.55933214561695));
#9360=CARTESIAN_POINT('Origin',(29.7,-16.2999999999999,8.));
#9361=CARTESIAN_POINT('',(29.7,-15.9999999999999,8.));
#9362=CARTESIAN_POINT('Origin',(29.7,16.2999999999999,8.));
#9363=CARTESIAN_POINT('',(29.7,15.9999999999999,4.));
#9364=CARTESIAN_POINT('',(29.7,15.9999999999999,8.));
#9365=CARTESIAN_POINT('Origin',(29.7,16.2999999999999,4.3));
#9366=CARTESIAN_POINT('Origin',(-29.7,-15.2999999999999,10.));
#9367=CARTESIAN_POINT('',(-29.7,-14.9999999999999,10.));
#9368=CARTESIAN_POINT('Origin',(29.7,7.49999999999996,4.3));
#9369=CARTESIAN_POINT('',(29.7,14.9999999999999,4.));
#9370=CARTESIAN_POINT('',(29.7,7.49999999999996,4.));
#9371=CARTESIAN_POINT('Origin',(29.7,15.2999999999999,4.3));
#9372=CARTESIAN_POINT('Origin',(29.7,15.2999999999999,10.));
#9373=CARTESIAN_POINT('',(29.7,14.9999999999999,10.));
#9374=CARTESIAN_POINT('Origin',(0.,15.9999999999999,4.));
#9375=CARTESIAN_POINT('',(0.,15.9999999999999,4.));
#9376=CARTESIAN_POINT('',(0.,15.9999999999999,-7.85933214561696));
#9377=CARTESIAN_POINT('Origin',(0.,14.9999999999999,4.));
#9378=CARTESIAN_POINT('',(0.,14.9999999999999,4.));
#9379=CARTESIAN_POINT('Origin',(0.,14.9999999999999,8.));
#9380=CARTESIAN_POINT('',(0.,14.9999999999999,8.));
#9381=CARTESIAN_POINT('Origin',(0.,-30.,8.));
#9382=CARTESIAN_POINT('',(0.,-14.9999999999999,8.));
#9383=CARTESIAN_POINT('Origin',(0.,-14.9999999999999,8.));
#9384=CARTESIAN_POINT('',(0.,-14.9999999999999,4.));
#9385=CARTESIAN_POINT('Origin',(0.,-15.9999999999999,-7.85933214561696));
#9386=CARTESIAN_POINT('',(0.,-15.9999999999999,-7.85933214561696));
#9387=CARTESIAN_POINT('Origin',(0.,-14.9999999999999,4.));
#9388=CARTESIAN_POINT('',(0.,-15.9999999999999,4.));
#9389=CARTESIAN_POINT('Origin',(0.,-15.9999999999999,4.));
#9390=CARTESIAN_POINT('Origin',(0.,27.9999999999999,-7.85933214561696));
#9391=CARTESIAN_POINT('Origin',(0.,-27.9999999999999,-7.85933214561696));
#9392=CARTESIAN_POINT('Origin',(0.,14.9999999999999,4.));
#9393=CARTESIAN_POINT('Origin',(0.,28.9999999999999,4.));
#9394=CARTESIAN_POINT('Origin',(0.,-14.9999999999999,4.));
#9395=CARTESIAN_POINT('Origin',(0.,-28.9999999999999,4.));
#9396=CARTESIAN_POINT('Origin',(0.,-30.,8.));
#9397=CARTESIAN_POINT('Origin',(0.,-30.,8.));
#9398=CARTESIAN_POINT('Origin',(0.,30.,8.));
#9399=CARTESIAN_POINT('Origin',(0.,-30.,16.));
#9400=CARTESIAN_POINT('Origin',(0.,15.9999999999999,-7.85933214561696));
#9401=CARTESIAN_POINT('Origin',(-14.1247849194883,-25.3746234146051,10.));
#9402=CARTESIAN_POINT('Origin',(-23.1247849194883,-6.37462341460511,10.));
#9403=CARTESIAN_POINT('Origin',(23.1247849194883,-6.37462341460511,10.));
#9404=CARTESIAN_POINT('Origin',(14.1247849194883,-25.3746234146051,10.));
#9405=CARTESIAN_POINT('Origin',(23.1247849194883,6.37462341460511,10.));
#9406=CARTESIAN_POINT('Origin',(23.1247849194883,15.3746234146051,10.));
#9407=CARTESIAN_POINT('Origin',(-23.1247849194883,-15.3746234146051,10.));
#9408=CARTESIAN_POINT('Origin',(-23.1247849194883,15.3746234146051,10.));
#9409=CARTESIAN_POINT('Origin',(-23.1247849194883,-25.3746234146051,10.));
#9410=CARTESIAN_POINT('Origin',(-23.1247849194883,6.37462341460511,10.));
#9411=CARTESIAN_POINT('Origin',(23.1247849194883,-15.3746234146051,10.));
#9412=CARTESIAN_POINT('Origin',(14.1247849194883,25.3746234146051,10.));
#9413=CARTESIAN_POINT('Origin',(23.1247849194883,-25.3746234146051,10.));
#9414=CARTESIAN_POINT('Origin',(23.1247849194883,25.3746234146051,10.));
#9415=CARTESIAN_POINT('Origin',(-23.1247849194883,25.3746234146051,10.));
#9416=CARTESIAN_POINT('Origin',(-14.1247849194883,25.3746234146051,10.));
#9417=CARTESIAN_POINT('',(0.,0.,0.));
#9418=CARTESIAN_POINT('Origin',(-13.3,-21.9999999999999,-1.92966607280848));
#9419=CARTESIAN_POINT('',(-13.,-21.9999999999999,-6.22966607280848));
#9420=CARTESIAN_POINT('Origin',(-13.,-21.9999999999999,-1.92966607280848));
#9421=CARTESIAN_POINT('',(-13.3,-21.9999999999999,-5.92966607280848));
#9422=CARTESIAN_POINT('Origin',(-13.3,-21.9999999999999,-6.22966607280848));
#9423=CARTESIAN_POINT('',(-13.3,-25.9999999999999,-1.92966607280848));
#9424=CARTESIAN_POINT('Origin',(-13.3,-21.9999999999999,-1.92966607280848));
#9425=CARTESIAN_POINT('Origin',(-13.3,-21.9999999999999,-1.92966607280848));
#9426=CARTESIAN_POINT('Origin',(-13.,-21.9999999999999,-1.92966607280848));
#9427=CARTESIAN_POINT('',(-13.,-21.9999999999999,2.77033392719152));
#9428=CARTESIAN_POINT('Origin',(-13.,-21.9999999999999,-1.92966607280848));
#9429=CARTESIAN_POINT('Origin',(-29.,-21.9999999999999,-1.92966607280848));
#9430=CARTESIAN_POINT('',(-28.7,-25.9999999999999,-1.92966607280848));
#9431=CARTESIAN_POINT('',(-29.,-25.9999999999999,-1.92966607280848));
#9432=CARTESIAN_POINT('',(-28.7,-21.9999999999999,2.07033392719152));
#9433=CARTESIAN_POINT('Origin',(-28.7,-21.9999999999999,-1.92966607280848));
#9434=CARTESIAN_POINT('Origin',(-28.7,-21.9999999999999,-1.92966607280848));
#9435=CARTESIAN_POINT('Origin',(-13.3,-21.9999999999999,-1.92966607280848));
#9436=CARTESIAN_POINT('',(-13.3,-21.9999999999999,3.07033392719152));
#9437=CARTESIAN_POINT('Origin',(-13.3,-21.9999999999999,2.77033392719152));
#9438=CARTESIAN_POINT('',(-13.3,-26.9999999999999,-1.92966607280848));
#9439=CARTESIAN_POINT('Origin',(-13.3,-21.9999999999999,-1.92966607280848));
#9440=CARTESIAN_POINT('Origin',(-13.3,-21.9999999999999,-1.92966607280848));
#9441=CARTESIAN_POINT('Origin',(-29.,-21.9999999999999,-1.92966607280848));
#9442=CARTESIAN_POINT('',(-28.7,-26.9999999999999,-1.92966607280848));
#9443=CARTESIAN_POINT('',(-29.,-26.9999999999999,-1.92966607280848));
#9444=CARTESIAN_POINT('',(-28.7,-21.9999999999999,-6.92966607280848));
#9445=CARTESIAN_POINT('Origin',(-28.7,-21.9999999999999,-1.92966607280848));
#9446=CARTESIAN_POINT('Origin',(-28.7,-21.9999999999999,-1.92966607280848));
#9447=CARTESIAN_POINT('Origin',(-28.7,-21.9999999999999,-1.92966607280848));
#9448=CARTESIAN_POINT('',(-29.,-21.9999999999999,2.37033392719152));
#9449=CARTESIAN_POINT('Origin',(-29.,-21.9999999999999,-1.92966607280848));
#9450=CARTESIAN_POINT('Origin',(-28.7,-21.9999999999999,2.37033392719152));
#9451=CARTESIAN_POINT('Origin',(-29.,-21.9999999999999,-1.92966607280848));
#9452=CARTESIAN_POINT('',(-29.,-21.9999999999999,-6.62966607280848));
#9453=CARTESIAN_POINT('Origin',(-29.,-21.9999999999999,-1.92966607280848));
#9454=CARTESIAN_POINT('Origin',(-28.7,-21.9999999999999,-1.92966607280848));
#9455=CARTESIAN_POINT('Origin',(-28.7,-21.9999999999999,-6.62966607280848));
#9456=CARTESIAN_POINT('',(0.,0.,0.));
#9457=CARTESIAN_POINT('Origin',(13.3,-21.9999999999999,-1.92966607280848));
#9458=CARTESIAN_POINT('',(13.,-21.9999999999999,-6.22966607280848));
#9459=CARTESIAN_POINT('Origin',(13.,-21.9999999999999,-1.92966607280848));
#9460=CARTESIAN_POINT('',(13.3,-21.9999999999999,-5.92966607280848));
#9461=CARTESIAN_POINT('Origin',(13.3,-21.9999999999999,-6.22966607280848));
#9462=CARTESIAN_POINT('',(13.3,-25.9999999999999,-1.92966607280848));
#9463=CARTESIAN_POINT('Origin',(13.3,-21.9999999999999,-1.92966607280848));
#9464=CARTESIAN_POINT('Origin',(13.3,-21.9999999999999,-1.92966607280848));
#9465=CARTESIAN_POINT('Origin',(13.,-21.9999999999999,-1.92966607280848));
#9466=CARTESIAN_POINT('',(13.,-21.9999999999999,2.77033392719152));
#9467=CARTESIAN_POINT('Origin',(13.,-21.9999999999999,-1.92966607280848));
#9468=CARTESIAN_POINT('Origin',(29.,-21.9999999999999,-1.92966607280848));
#9469=CARTESIAN_POINT('',(28.7,-25.9999999999999,-1.92966607280848));
#9470=CARTESIAN_POINT('',(29.,-25.9999999999999,-1.92966607280848));
#9471=CARTESIAN_POINT('',(28.7,-21.9999999999999,2.07033392719152));
#9472=CARTESIAN_POINT('Origin',(28.7,-21.9999999999999,-1.92966607280848));
#9473=CARTESIAN_POINT('Origin',(28.7,-21.9999999999999,-1.92966607280848));
#9474=CARTESIAN_POINT('Origin',(13.3,-21.9999999999999,-1.92966607280848));
#9475=CARTESIAN_POINT('',(13.3,-21.9999999999999,3.07033392719152));
#9476=CARTESIAN_POINT('Origin',(13.3,-21.9999999999999,2.77033392719152));
#9477=CARTESIAN_POINT('',(13.3,-26.9999999999999,-1.92966607280848));
#9478=CARTESIAN_POINT('Origin',(13.3,-21.9999999999999,-1.92966607280848));
#9479=CARTESIAN_POINT('Origin',(13.3,-21.9999999999999,-1.92966607280848));
#9480=CARTESIAN_POINT('Origin',(29.,-21.9999999999999,-1.92966607280848));
#9481=CARTESIAN_POINT('',(28.7,-26.9999999999999,-1.92966607280848));
#9482=CARTESIAN_POINT('',(29.,-26.9999999999999,-1.92966607280848));
#9483=CARTESIAN_POINT('',(28.7,-21.9999999999999,-6.92966607280848));
#9484=CARTESIAN_POINT('Origin',(28.7,-21.9999999999999,-1.92966607280848));
#9485=CARTESIAN_POINT('Origin',(28.7,-21.9999999999999,-1.92966607280848));
#9486=CARTESIAN_POINT('Origin',(28.7,-21.9999999999999,-1.92966607280848));
#9487=CARTESIAN_POINT('',(29.,-21.9999999999999,2.37033392719152));
#9488=CARTESIAN_POINT('Origin',(29.,-21.9999999999999,-1.92966607280848));
#9489=CARTESIAN_POINT('Origin',(28.7,-21.9999999999999,2.37033392719152));
#9490=CARTESIAN_POINT('Origin',(29.,-21.9999999999999,-1.92966607280848));
#9491=CARTESIAN_POINT('',(29.,-21.9999999999999,-6.62966607280848));
#9492=CARTESIAN_POINT('Origin',(29.,-21.9999999999999,-1.92966607280848));
#9493=CARTESIAN_POINT('Origin',(28.7,-21.9999999999999,-1.92966607280848));
#9494=CARTESIAN_POINT('Origin',(28.7,-21.9999999999999,-6.62966607280848));
#9495=CARTESIAN_POINT('',(0.,0.,0.));
#9496=CARTESIAN_POINT('Origin',(133.037195913696,35.,-10.3));
#9497=CARTESIAN_POINT('',(135.037195913696,35.,-10.3));
#9498=CARTESIAN_POINT('Origin',(133.037195913696,35.,-10.3));
#9499=CARTESIAN_POINT('',(135.337195913696,35.,-10.));
#9500=CARTESIAN_POINT('Origin',(135.337195913696,35.,-10.3));
#9501=CARTESIAN_POINT('Origin',(133.037195913696,35.,-10.));
#9502=CARTESIAN_POINT('Origin',(137.,35.,-10.));
#9503=CARTESIAN_POINT('',(144.7,39.7,-10.));
#9504=CARTESIAN_POINT('',(129.3,39.7,-10.));
#9505=CARTESIAN_POINT('',(141.,39.7,-10.));
#9506=CARTESIAN_POINT('',(129.3,30.3,-10.));
#9507=CARTESIAN_POINT('',(129.3,2.5,-10.));
#9508=CARTESIAN_POINT('',(144.7,30.3,-10.));
#9509=CARTESIAN_POINT('',(133.,30.3,-10.));
#9510=CARTESIAN_POINT('',(144.7,32.5,-10.));
#9511=CARTESIAN_POINT('',(143.262804086304,35.,-10.));
#9512=CARTESIAN_POINT('Origin',(140.962804086304,35.,-10.));
#9513=CARTESIAN_POINT('Origin',(133.037195913696,35.,-16.));
#9514=CARTESIAN_POINT('',(135.037195913696,35.,-16.));
#9515=CARTESIAN_POINT('',(135.037195913696,35.,-16.));
#9516=CARTESIAN_POINT('Origin',(133.037195913696,35.,-16.));
#9517=CARTESIAN_POINT('Origin',(140.962804086304,35.,-10.3));
#9518=CARTESIAN_POINT('',(142.962804086304,35.,-10.3));
#9519=CARTESIAN_POINT('Origin',(140.962804086304,35.,-10.3));
#9520=CARTESIAN_POINT('Origin',(143.262804086304,35.,-10.3));
#9521=CARTESIAN_POINT('Origin',(140.962804086304,35.,-16.));
#9522=CARTESIAN_POINT('',(142.962804086304,35.,-16.));
#9523=CARTESIAN_POINT('',(142.962804086304,35.,-16.));
#9524=CARTESIAN_POINT('Origin',(140.962804086304,35.,-16.));
#9525=CARTESIAN_POINT('Origin',(133.037195913696,-35.,-10.3));
#9526=CARTESIAN_POINT('',(130.737195913696,-35.,-10.));
#9527=CARTESIAN_POINT('Origin',(133.037195913696,-35.,-10.));
#9528=CARTESIAN_POINT('',(131.037195913696,-35.,-10.3));
#9529=CARTESIAN_POINT('Origin',(130.737195913696,-35.,-10.3));
#9530=CARTESIAN_POINT('',(135.037195913696,-35.,-10.3));
#9531=CARTESIAN_POINT('Origin',(133.037195913696,-35.,-10.3));
#9532=CARTESIAN_POINT('Origin',(133.037195913696,-35.,-10.3));
#9533=CARTESIAN_POINT('Origin',(137.,-35.,-10.));
#9534=CARTESIAN_POINT('',(144.7,-30.3,-10.));
#9535=CARTESIAN_POINT('',(129.3,-30.3,-10.));
#9536=CARTESIAN_POINT('',(141.,-30.3,-10.));
#9537=CARTESIAN_POINT('',(129.3,-39.7,-10.));
#9538=CARTESIAN_POINT('',(129.3,-32.5,-10.));
#9539=CARTESIAN_POINT('',(144.7,-39.7,-10.));
#9540=CARTESIAN_POINT('',(141.,-39.7,-10.));
#9541=CARTESIAN_POINT('',(144.7,-2.5,-10.));
#9542=CARTESIAN_POINT('',(138.662804086304,-35.,-10.));
#9543=CARTESIAN_POINT('Origin',(140.962804086304,-35.,-10.));
#9544=CARTESIAN_POINT('Origin',(133.037195913696,-35.,-16.));
#9545=CARTESIAN_POINT('',(135.037195913696,-35.,-16.));
#9546=CARTESIAN_POINT('',(135.037195913696,-35.,-16.));
#9547=CARTESIAN_POINT('Origin',(133.037195913696,-35.,-16.));
#9548=CARTESIAN_POINT('Origin',(140.962804086304,-35.,-10.3));
#9549=CARTESIAN_POINT('',(138.962804086304,-35.,-10.3));
#9550=CARTESIAN_POINT('Origin',(138.662804086304,-35.,-10.3));
#9551=CARTESIAN_POINT('',(142.962804086304,-35.,-10.3));
#9552=CARTESIAN_POINT('Origin',(140.962804086304,-35.,-10.3));
#9553=CARTESIAN_POINT('Origin',(140.962804086304,-35.,-10.3));
#9554=CARTESIAN_POINT('Origin',(140.962804086304,-35.,-16.));
#9555=CARTESIAN_POINT('',(142.962804086304,-35.,-16.));
#9556=CARTESIAN_POINT('',(142.962804086304,-35.,-16.));
#9557=CARTESIAN_POINT('Origin',(140.962804086304,-35.,-16.));
#9558=CARTESIAN_POINT('Origin',(144.7,-39.7,-15.7));
#9559=CARTESIAN_POINT('',(145.,-39.7,-15.7));
#9560=CARTESIAN_POINT('',(144.7,-40.,-15.7));
#9561=CARTESIAN_POINT('Origin',(144.7,-39.7,-15.7));
#9562=CARTESIAN_POINT('',(144.7,-39.7,-16.));
#9563=CARTESIAN_POINT('Origin',(144.7,-39.7,-15.7));
#9564=CARTESIAN_POINT('Origin',(144.7,-39.7,-15.7));
#9565=CARTESIAN_POINT('Origin',(129.3,-39.7,-15.7));
#9566=CARTESIAN_POINT('',(129.3,-39.7,-16.));
#9567=CARTESIAN_POINT('',(129.3,-40.,-15.7));
#9568=CARTESIAN_POINT('Origin',(129.3,-39.7,-15.7));
#9569=CARTESIAN_POINT('',(129.,-39.7,-15.7));
#9570=CARTESIAN_POINT('Origin',(129.3,-39.7,-15.7));
#9571=CARTESIAN_POINT('Origin',(129.3,-39.7,-15.7));
#9572=CARTESIAN_POINT('Origin',(144.7,39.7,-15.7));
#9573=CARTESIAN_POINT('',(144.7,39.7,-16.));
#9574=CARTESIAN_POINT('',(144.7,40.,-15.7));
#9575=CARTESIAN_POINT('Origin',(144.7,39.7,-15.7));
#9576=CARTESIAN_POINT('',(145.,39.7,-15.7));
#9577=CARTESIAN_POINT('Origin',(144.7,39.7,-15.7));
#9578=CARTESIAN_POINT('Origin',(144.7,39.7,-15.7));
#9579=CARTESIAN_POINT('Origin',(144.7,15.,-15.7));
#9580=CARTESIAN_POINT('',(145.,15.,-15.7));
#9581=CARTESIAN_POINT('',(144.7,15.,-16.));
#9582=CARTESIAN_POINT('Origin',(144.7,-39.7,-10.3));
#9583=CARTESIAN_POINT('',(145.,-39.7,-10.3));
#9584=CARTESIAN_POINT('Origin',(144.7,-39.7,-10.3));
#9585=CARTESIAN_POINT('',(144.7,-40.,-10.3));
#9586=CARTESIAN_POINT('Origin',(144.7,-39.7,-10.3));
#9587=CARTESIAN_POINT('Origin',(144.7,-39.7,-10.3));
#9588=CARTESIAN_POINT('Origin',(144.7,-39.7,-8.));
#9589=CARTESIAN_POINT('',(144.7,-40.,-8.));
#9590=CARTESIAN_POINT('',(145.,-39.7,-8.));
#9591=CARTESIAN_POINT('Origin',(129.3,39.7,-15.7));
#9592=CARTESIAN_POINT('',(129.,39.7,-15.7));
#9593=CARTESIAN_POINT('',(129.3,40.,-15.7));
#9594=CARTESIAN_POINT('Origin',(129.3,39.7,-15.7));
#9595=CARTESIAN_POINT('',(129.3,39.7,-16.));
#9596=CARTESIAN_POINT('Origin',(129.3,39.7,-15.7));
#9597=CARTESIAN_POINT('Origin',(129.3,39.7,-15.7));
#9598=CARTESIAN_POINT('Origin',(129.3,-15.,-15.7));
#9599=CARTESIAN_POINT('',(129.3,-15.,-16.));
#9600=CARTESIAN_POINT('',(129.,-15.,-15.7));
#9601=CARTESIAN_POINT('Origin',(141.,39.7,-15.7));
#9602=CARTESIAN_POINT('',(141.,39.7,-16.));
#9603=CARTESIAN_POINT('',(141.,40.,-15.7));
#9604=CARTESIAN_POINT('Origin',(129.3,-39.7,-10.3));
#9605=CARTESIAN_POINT('',(129.3,-40.,-10.3));
#9606=CARTESIAN_POINT('Origin',(129.3,-39.7,-10.3));
#9607=CARTESIAN_POINT('',(129.,-39.7,-10.3));
#9608=CARTESIAN_POINT('Origin',(129.3,-39.7,-10.3));
#9609=CARTESIAN_POINT('Origin',(129.3,-39.7,-10.3));
#9610=CARTESIAN_POINT('Origin',(129.3,-39.7,-8.));
#9611=CARTESIAN_POINT('',(129.,-39.7,-8.));
#9612=CARTESIAN_POINT('',(129.3,-40.,-8.));
#9613=CARTESIAN_POINT('Origin',(144.7,39.7,-10.3));
#9614=CARTESIAN_POINT('',(145.,39.7,-10.3));
#9615=CARTESIAN_POINT('',(144.7,40.,-10.3));
#9616=CARTESIAN_POINT('Origin',(144.7,39.7,-10.3));
#9617=CARTESIAN_POINT('Origin',(144.7,39.7,-10.3));
#9618=CARTESIAN_POINT('Origin',(144.7,39.7,-10.3));
#9619=CARTESIAN_POINT('Origin',(144.7,-30.3,-9.7));
#9620=CARTESIAN_POINT('',(144.7,-30.,-9.7));
#9621=CARTESIAN_POINT('Origin',(144.7,-30.3,-9.7));
#9622=CARTESIAN_POINT('',(145.,-30.3,-10.3));
#9623=CARTESIAN_POINT('Origin',(144.7,-30.3,-10.3));
#9624=CARTESIAN_POINT('',(145.,-29.7,-9.7));
#9625=CARTESIAN_POINT('Origin',(145.,-30.3,-9.7));
#9626=CARTESIAN_POINT('Origin',(144.7,-29.7,-9.7));
#9627=CARTESIAN_POINT('Origin',(129.3,39.7,-10.3));
#9628=CARTESIAN_POINT('',(129.3,40.,-10.3));
#9629=CARTESIAN_POINT('',(129.,39.7,-10.3));
#9630=CARTESIAN_POINT('Origin',(129.3,39.7,-10.3));
#9631=CARTESIAN_POINT('Origin',(129.3,39.7,-10.3));
#9632=CARTESIAN_POINT('Origin',(129.3,39.7,-10.3));
#9633=CARTESIAN_POINT('Origin',(141.,39.7,-10.3));
#9634=CARTESIAN_POINT('',(141.,40.,-10.3));
#9635=CARTESIAN_POINT('Origin',(129.3,-30.3,-9.7));
#9636=CARTESIAN_POINT('',(129.,-30.3,-10.3));
#9637=CARTESIAN_POINT('',(129.,-29.7,-9.7));
#9638=CARTESIAN_POINT('Origin',(129.,-30.3,-9.7));
#9639=CARTESIAN_POINT('Origin',(129.3,-30.3,-10.3));
#9640=CARTESIAN_POINT('',(129.3,-30.,-9.7));
#9641=CARTESIAN_POINT('Origin',(129.3,-30.3,-9.7));
#9642=CARTESIAN_POINT('Origin',(129.3,-29.7,-9.7));
#9643=CARTESIAN_POINT('Origin',(144.7,30.3,-9.7));
#9644=CARTESIAN_POINT('',(145.,30.3,-10.3));
#9645=CARTESIAN_POINT('',(145.,29.7,-9.7));
#9646=CARTESIAN_POINT('Origin',(145.,30.3,-9.7));
#9647=CARTESIAN_POINT('Origin',(144.7,30.3,-10.3));
#9648=CARTESIAN_POINT('',(144.7,30.,-9.7));
#9649=CARTESIAN_POINT('Origin',(144.7,30.3,-9.7));
#9650=CARTESIAN_POINT('Origin',(144.7,29.7,-9.7));
#9651=CARTESIAN_POINT('Origin',(144.7,-29.7,15.7));
#9652=CARTESIAN_POINT('',(145.,-29.7,15.7));
#9653=CARTESIAN_POINT('',(144.7,-29.7,16.));
#9654=CARTESIAN_POINT('Origin',(144.7,-29.7,15.7));
#9655=CARTESIAN_POINT('',(144.7,-30.,15.7));
#9656=CARTESIAN_POINT('Origin',(144.7,-29.7,15.7));
#9657=CARTESIAN_POINT('Origin',(144.7,-29.7,15.7));
#9658=CARTESIAN_POINT('Origin',(144.7,-29.7,0.));
#9659=CARTESIAN_POINT('',(145.,-29.7,0.));
#9660=CARTESIAN_POINT('',(144.7,-30.,0.));
#9661=CARTESIAN_POINT('Origin',(129.3,30.3,-9.7));
#9662=CARTESIAN_POINT('',(129.3,30.,-9.7));
#9663=CARTESIAN_POINT('Origin',(129.3,30.3,-9.7));
#9664=CARTESIAN_POINT('',(129.,30.3,-10.3));
#9665=CARTESIAN_POINT('Origin',(129.3,30.3,-10.3));
#9666=CARTESIAN_POINT('',(129.,29.7,-9.7));
#9667=CARTESIAN_POINT('Origin',(129.,30.3,-9.7));
#9668=CARTESIAN_POINT('Origin',(129.3,29.7,-9.7));
#9669=CARTESIAN_POINT('Origin',(129.3,-29.7,15.7));
#9670=CARTESIAN_POINT('',(129.3,-30.,15.7));
#9671=CARTESIAN_POINT('',(129.3,-29.7,16.));
#9672=CARTESIAN_POINT('Origin',(129.3,-29.7,15.7));
#9673=CARTESIAN_POINT('',(129.,-29.7,15.7));
#9674=CARTESIAN_POINT('Origin',(129.3,-29.7,15.7));
#9675=CARTESIAN_POINT('Origin',(129.3,-29.7,15.7));
#9676=CARTESIAN_POINT('Origin',(129.3,-29.7,0.));
#9677=CARTESIAN_POINT('',(129.,-29.7,0.));
#9678=CARTESIAN_POINT('',(129.3,-30.,0.));
#9679=CARTESIAN_POINT('Origin',(144.7,29.7,15.7));
#9680=CARTESIAN_POINT('',(144.7,30.,15.7));
#9681=CARTESIAN_POINT('',(144.7,29.7,16.));
#9682=CARTESIAN_POINT('Origin',(144.7,29.7,15.7));
#9683=CARTESIAN_POINT('',(145.,29.7,15.7));
#9684=CARTESIAN_POINT('Origin',(144.7,29.7,15.7));
#9685=CARTESIAN_POINT('Origin',(144.7,29.7,15.7));
#9686=CARTESIAN_POINT('Origin',(144.7,29.7,0.));
#9687=CARTESIAN_POINT('',(145.,29.7,0.));
#9688=CARTESIAN_POINT('',(144.7,30.,0.));
#9689=CARTESIAN_POINT('Origin',(144.7,-22.7999999999999,15.7));
#9690=CARTESIAN_POINT('',(145.,-22.7999999999999,15.7));
#9691=CARTESIAN_POINT('',(144.7,-22.4999999999999,15.7));
#9692=CARTESIAN_POINT('Origin',(144.7,-22.7999999999999,15.7));
#9693=CARTESIAN_POINT('',(144.7,-22.7999999999999,16.));
#9694=CARTESIAN_POINT('Origin',(144.7,-22.7999999999999,15.7));
#9695=CARTESIAN_POINT('Origin',(144.7,-22.7999999999999,15.7));
#9696=CARTESIAN_POINT('Origin',(144.7,15.,15.7));
#9697=CARTESIAN_POINT('',(145.,15.,15.7));
#9698=CARTESIAN_POINT('',(144.7,15.,16.));
#9699=CARTESIAN_POINT('Origin',(129.3,29.7,15.7));
#9700=CARTESIAN_POINT('',(129.,29.7,15.7));
#9701=CARTESIAN_POINT('',(129.3,29.7,16.));
#9702=CARTESIAN_POINT('Origin',(129.3,29.7,15.7));
#9703=CARTESIAN_POINT('',(129.3,30.,15.7));
#9704=CARTESIAN_POINT('Origin',(129.3,29.7,15.7));
#9705=CARTESIAN_POINT('Origin',(129.3,29.7,15.7));
#9706=CARTESIAN_POINT('Origin',(129.3,29.7,0.));
#9707=CARTESIAN_POINT('',(129.3,30.,0.));
#9708=CARTESIAN_POINT('',(129.,29.7,0.));
#9709=CARTESIAN_POINT('Origin',(133.,29.7,15.7));
#9710=CARTESIAN_POINT('',(133.,30.,15.7));
#9711=CARTESIAN_POINT('',(133.,29.7,16.));
#9712=CARTESIAN_POINT('Origin',(129.3,-22.7999999999999,15.7));
#9713=CARTESIAN_POINT('',(129.,-22.7999999999999,15.7));
#9714=CARTESIAN_POINT('',(129.3,-22.7999999999999,16.));
#9715=CARTESIAN_POINT('Origin',(129.3,-22.7999999999999,15.7));
#9716=CARTESIAN_POINT('',(129.3,-22.4999999999999,15.7));
#9717=CARTESIAN_POINT('Origin',(129.3,-22.7999999999999,15.7));
#9718=CARTESIAN_POINT('Origin',(129.3,-22.7999999999999,15.7));
#9719=CARTESIAN_POINT('Origin',(144.7,22.7999999999999,15.7));
#9720=CARTESIAN_POINT('',(144.7,22.4999999999999,15.7));
#9721=CARTESIAN_POINT('',(145.,22.7999999999999,15.7));
#9722=CARTESIAN_POINT('Origin',(144.7,22.7999999999999,15.7));
#9723=CARTESIAN_POINT('',(144.7,22.7999999999999,16.));
#9724=CARTESIAN_POINT('Origin',(144.7,22.7999999999999,15.7));
#9725=CARTESIAN_POINT('Origin',(144.7,22.7999999999999,15.7));
#9726=CARTESIAN_POINT('Origin',(144.7,-22.7999999999999,8.));
#9727=CARTESIAN_POINT('',(145.,-22.7999999999999,2.29525996204705));
#9728=CARTESIAN_POINT('',(145.,-22.7999999999999,8.));
#9729=CARTESIAN_POINT('',(144.7,-22.4999999999999,2.03896089378841));
#9730=CARTESIAN_POINT('Ctrl Pts',(144.7,-22.4999999999999,2.03896089378841));
#9731=CARTESIAN_POINT('Ctrl Pts',(144.729707021216,-22.4999999999999,2.03896089378841));
#9732=CARTESIAN_POINT('Ctrl Pts',(144.758777673282,-22.5044062942651,2.04285168076791));
#9733=CARTESIAN_POINT('Ctrl Pts',(144.817440852233,-22.5220432289933,2.05836227087722));
#9734=CARTESIAN_POINT('Ctrl Pts',(144.845615509175,-22.5359942380498,2.07060652861162));
#9735=CARTESIAN_POINT('Ctrl Pts',(144.902101216584,-22.5749600084548,2.10457296342855));
#9736=CARTESIAN_POINT('Ctrl Pts',(144.927927434013,-22.6017796731997,2.12780612534896));
#9737=CARTESIAN_POINT('Ctrl Pts',(144.964853191741,-22.6558870245156,2.17419410934337));
#9738=CARTESIAN_POINT('Ctrl Pts',(144.977648024164,-22.6827478353212,2.19704892778962));
#9739=CARTESIAN_POINT('Ctrl Pts',(144.995183002528,-22.7387435986925,2.24427435404391));
#9740=CARTESIAN_POINT('Ctrl Pts',(144.999750204092,-22.768135790235,2.26885093228759));
#9741=CARTESIAN_POINT('Ctrl Pts',(144.999996676585,-22.7983695157586,2.29390907943587));
#9742=CARTESIAN_POINT('Ctrl Pts',(145.,-22.7991847191594,2.29458456964534));
#9743=CARTESIAN_POINT('Ctrl Pts',(145.,-22.7999999999999,2.29525996204705));
#9744=CARTESIAN_POINT('',(144.7,-22.4999999999999,8.));
#9745=CARTESIAN_POINT('Origin',(129.3,22.7999999999999,15.7));
#9746=CARTESIAN_POINT('',(129.,22.7999999999999,15.7));
#9747=CARTESIAN_POINT('',(129.3,22.4999999999999,15.7));
#9748=CARTESIAN_POINT('Origin',(129.3,22.7999999999999,15.7));
#9749=CARTESIAN_POINT('',(129.3,22.7999999999999,16.));
#9750=CARTESIAN_POINT('Origin',(129.3,22.7999999999999,15.7));
#9751=CARTESIAN_POINT('Origin',(129.3,22.7999999999999,15.7));
#9752=CARTESIAN_POINT('Origin',(129.3,-15.,15.7));
#9753=CARTESIAN_POINT('',(129.,-15.,15.7));
#9754=CARTESIAN_POINT('',(129.3,-15.,16.));
#9755=CARTESIAN_POINT('Origin',(141.,22.7999999999999,15.7));
#9756=CARTESIAN_POINT('',(141.,22.4999999999999,15.7));
#9757=CARTESIAN_POINT('',(141.,22.7999999999999,16.));
#9758=CARTESIAN_POINT('Origin',(129.3,-22.7999999999999,8.));
#9759=CARTESIAN_POINT('',(129.3,-22.4999999999999,2.03896089378841));
#9760=CARTESIAN_POINT('',(129.3,-22.4999999999999,8.));
#9761=CARTESIAN_POINT('',(129.,-22.7999999999999,2.29525996204705));
#9762=CARTESIAN_POINT('Ctrl Pts',(129.,-22.7999999999999,2.29525996204705));
#9763=CARTESIAN_POINT('Ctrl Pts',(129.,-22.7991847191433,2.29458456963201));
#9764=CARTESIAN_POINT('Ctrl Pts',(129.000003323414,-22.798369515774,2.29390907945453));
#9765=CARTESIAN_POINT('Ctrl Pts',(129.000249795909,-22.7681357900482,2.26885093208373));
#9766=CARTESIAN_POINT('Ctrl Pts',(129.004816997483,-22.7387435986578,2.24427435401478));
#9767=CARTESIAN_POINT('Ctrl Pts',(129.022351975836,-22.6827478353226,2.19704892779083));
#9768=CARTESIAN_POINT('Ctrl Pts',(129.035146808259,-22.6558870245162,2.17419410934394));
#9769=CARTESIAN_POINT('Ctrl Pts',(129.072072565987,-22.6017796731997,2.12780612534895));
#9770=CARTESIAN_POINT('Ctrl Pts',(129.097898783416,-22.5749600084547,2.10457296342854));
#9771=CARTESIAN_POINT('Ctrl Pts',(129.154384490824,-22.5359942380497,2.07060652861162));
#9772=CARTESIAN_POINT('Ctrl Pts',(129.182559147767,-22.5220432289933,2.05836227087722));
#9773=CARTESIAN_POINT('Ctrl Pts',(129.241222326718,-22.5044062942651,2.04285168076791));
#9774=CARTESIAN_POINT('Ctrl Pts',(129.270292978784,-22.4999999999999,2.03896089378841));
#9775=CARTESIAN_POINT('Ctrl Pts',(129.3,-22.4999999999999,2.03896089378841));
#9776=CARTESIAN_POINT('',(129.,-22.7999999999999,8.));
#9777=CARTESIAN_POINT('Origin',(144.7,22.7999999999999,8.));
#9778=CARTESIAN_POINT('',(144.7,22.4999999999999,2.03896089378841));
#9779=CARTESIAN_POINT('',(144.7,22.4999999999999,8.));
#9780=CARTESIAN_POINT('',(145.,22.7999999999999,2.29525996204705));
#9781=CARTESIAN_POINT('Ctrl Pts',(145.,22.7999999999999,2.29525996204705));
#9782=CARTESIAN_POINT('Ctrl Pts',(145.,22.7991847191433,2.29458456963199));
#9783=CARTESIAN_POINT('Ctrl Pts',(144.999996676586,22.798369515774,2.29390907945454));
#9784=CARTESIAN_POINT('Ctrl Pts',(144.99975020409,22.768135790048,2.26885093208354));
#9785=CARTESIAN_POINT('Ctrl Pts',(144.995183002517,22.7387435986577,2.24427435401474));
#9786=CARTESIAN_POINT('Ctrl Pts',(144.977648024164,22.6827478353226,2.19704892779082));
#9787=CARTESIAN_POINT('Ctrl Pts',(144.964853191741,22.6558870245162,2.17419410934393));
#9788=CARTESIAN_POINT('Ctrl Pts',(144.927927434013,22.6017796731997,2.12780612534896));
#9789=CARTESIAN_POINT('Ctrl Pts',(144.902101216584,22.5749600084548,2.10457296342855));
#9790=CARTESIAN_POINT('Ctrl Pts',(144.845615509175,22.5359942380498,2.07060652861164));
#9791=CARTESIAN_POINT('Ctrl Pts',(144.817440852233,22.5220432289933,2.05836227087723));
#9792=CARTESIAN_POINT('Ctrl Pts',(144.758777673282,22.5044062942651,2.04285168076791));
#9793=CARTESIAN_POINT('Ctrl Pts',(144.729707021216,22.4999999999999,2.03896089378841));
#9794=CARTESIAN_POINT('Ctrl Pts',(144.7,22.4999999999999,2.03896089378841));
#9795=CARTESIAN_POINT('',(145.,22.7999999999999,8.));
#9796=CARTESIAN_POINT('Origin',(129.3,22.7999999999999,8.));
#9797=CARTESIAN_POINT('',(129.,22.7999999999999,2.29525996204705));
#9798=CARTESIAN_POINT('',(129.,22.7999999999999,8.));
#9799=CARTESIAN_POINT('',(129.3,22.4999999999999,2.03896089378841));
#9800=CARTESIAN_POINT('Ctrl Pts',(129.3,22.4999999999999,2.03896089378841));
#9801=CARTESIAN_POINT('Ctrl Pts',(129.270292978784,22.4999999999999,2.03896089378841));
#9802=CARTESIAN_POINT('Ctrl Pts',(129.241222326718,22.5044062942651,2.04285168076791));
#9803=CARTESIAN_POINT('Ctrl Pts',(129.182559147767,22.5220432289932,2.05836227087722));
#9804=CARTESIAN_POINT('Ctrl Pts',(129.154384490824,22.5359942380497,2.07060652861162));
#9805=CARTESIAN_POINT('Ctrl Pts',(129.097898783416,22.5749600084547,2.10457296342855));
#9806=CARTESIAN_POINT('Ctrl Pts',(129.072072565987,22.6017796731997,2.12780612534895));
#9807=CARTESIAN_POINT('Ctrl Pts',(129.035146808259,22.6558870245162,2.17419410934394));
#9808=CARTESIAN_POINT('Ctrl Pts',(129.022351975836,22.6827478353226,2.19704892779082));
#9809=CARTESIAN_POINT('Ctrl Pts',(129.004816997483,22.7387435986577,2.24427435401479));
#9810=CARTESIAN_POINT('Ctrl Pts',(129.000249795909,22.7681357900482,2.26885093208374));
#9811=CARTESIAN_POINT('Ctrl Pts',(129.000003323414,22.798369515774,2.29390907945453));
#9812=CARTESIAN_POINT('Ctrl Pts',(129.,22.7991847191433,2.29458456963201));
#9813=CARTESIAN_POINT('Ctrl Pts',(129.,22.7999999999999,2.29525996204705));
#9814=CARTESIAN_POINT('',(129.3,22.4999999999999,8.));
#9815=CARTESIAN_POINT('Origin',(144.7,-21.1999999999999,15.7));
#9816=CARTESIAN_POINT('',(144.7,-21.4999999999999,15.7));
#9817=CARTESIAN_POINT('',(145.,-21.1999999999999,15.7));
#9818=CARTESIAN_POINT('Origin',(144.7,-21.1999999999999,15.7));
#9819=CARTESIAN_POINT('',(144.7,-21.1999999999999,16.));
#9820=CARTESIAN_POINT('Origin',(144.7,-21.1999999999999,15.7));
#9821=CARTESIAN_POINT('Origin',(144.7,-21.1999999999999,15.7));
#9822=CARTESIAN_POINT('Origin',(129.3,-21.1999999999999,15.7));
#9823=CARTESIAN_POINT('',(129.,-21.1999999999999,15.7));
#9824=CARTESIAN_POINT('',(129.3,-21.4999999999999,15.7));
#9825=CARTESIAN_POINT('Origin',(129.3,-21.1999999999999,15.7));
#9826=CARTESIAN_POINT('',(129.3,-21.1999999999999,16.));
#9827=CARTESIAN_POINT('Origin',(129.3,-21.1999999999999,15.7));
#9828=CARTESIAN_POINT('Origin',(129.3,-21.1999999999999,15.7));
#9829=CARTESIAN_POINT('Origin',(144.7,21.1999999999999,15.7));
#9830=CARTESIAN_POINT('',(145.,21.1999999999999,15.7));
#9831=CARTESIAN_POINT('',(144.7,21.4999999999999,15.7));
#9832=CARTESIAN_POINT('Origin',(144.7,21.1999999999999,15.7));
#9833=CARTESIAN_POINT('',(144.7,21.1999999999999,16.));
#9834=CARTESIAN_POINT('Origin',(144.7,21.1999999999999,15.7));
#9835=CARTESIAN_POINT('Origin',(144.7,21.1999999999999,15.7));
#9836=CARTESIAN_POINT('Origin',(144.7,15.,15.7));
#9837=CARTESIAN_POINT('',(145.,15.,15.7));
#9838=CARTESIAN_POINT('',(144.7,15.,16.));
#9839=CARTESIAN_POINT('Origin',(129.3,21.1999999999999,15.7));
#9840=CARTESIAN_POINT('',(129.,21.1999999999999,15.7));
#9841=CARTESIAN_POINT('',(129.3,21.1999999999999,16.));
#9842=CARTESIAN_POINT('Origin',(129.3,21.1999999999999,15.7));
#9843=CARTESIAN_POINT('',(129.3,21.4999999999999,15.7));
#9844=CARTESIAN_POINT('Origin',(129.3,21.1999999999999,15.7));
#9845=CARTESIAN_POINT('Origin',(129.3,21.1999999999999,15.7));
#9846=CARTESIAN_POINT('Origin',(129.3,21.1999999999999,1.01948044689421));
#9847=CARTESIAN_POINT('',(129.3,21.4999999999999,2.03896089378841));
#9848=CARTESIAN_POINT('',(129.3,21.4999999999999,1.01948044689421));
#9849=CARTESIAN_POINT('',(129.,21.1999999999999,2.29525996204705));
#9850=CARTESIAN_POINT('Ctrl Pts',(129.,21.1999999999999,2.29525996204705));
#9851=CARTESIAN_POINT('Ctrl Pts',(129.,21.2008152808565,2.29458456963201));
#9852=CARTESIAN_POINT('Ctrl Pts',(129.000003323414,21.2016304842259,2.29390907945453));
#9853=CARTESIAN_POINT('Ctrl Pts',(129.000249795909,21.2318642099517,2.26885093208371));
#9854=CARTESIAN_POINT('Ctrl Pts',(129.004816997483,21.2612564013421,2.24427435401476));
#9855=CARTESIAN_POINT('Ctrl Pts',(129.022351975836,21.3172521646773,2.19704892779083));
#9856=CARTESIAN_POINT('Ctrl Pts',(129.035146808259,21.3441129754836,2.17419410934394));
#9857=CARTESIAN_POINT('Ctrl Pts',(129.072072565987,21.3982203268002,2.12780612534896));
#9858=CARTESIAN_POINT('Ctrl Pts',(129.097898783416,21.4250399915451,2.10457296342855));
#9859=CARTESIAN_POINT('Ctrl Pts',(129.154384490824,21.4640057619501,2.07060652861162));
#9860=CARTESIAN_POINT('Ctrl Pts',(129.182559147767,21.4779567710066,2.05836227087723));
#9861=CARTESIAN_POINT('Ctrl Pts',(129.241222326718,21.4955937057348,2.04285168076791));
#9862=CARTESIAN_POINT('Ctrl Pts',(129.270292978784,21.4999999999999,2.03896089378841));
#9863=CARTESIAN_POINT('Ctrl Pts',(129.3,21.4999999999999,2.03896089378841));
#9864=CARTESIAN_POINT('',(129.,21.1999999999999,1.01948044689421));
#9865=CARTESIAN_POINT('Origin',(141.,21.1999999999999,15.7));
#9866=CARTESIAN_POINT('',(141.,21.4999999999999,15.7));
#9867=CARTESIAN_POINT('',(141.,21.1999999999999,16.));
#9868=CARTESIAN_POINT('Origin',(129.3,-15.,15.7));
#9869=CARTESIAN_POINT('',(129.,-15.,15.7));
#9870=CARTESIAN_POINT('',(129.3,-15.,16.));
#9871=CARTESIAN_POINT('Origin',(144.7,21.1999999999999,1.01948044689421));
#9872=CARTESIAN_POINT('',(145.,21.1999999999999,2.29525996204705));
#9873=CARTESIAN_POINT('',(145.,21.1999999999999,1.01948044689421));
#9874=CARTESIAN_POINT('',(144.7,21.4999999999999,2.03896089378841));
#9875=CARTESIAN_POINT('Ctrl Pts',(144.7,21.4999999999999,2.03896089378841));
#9876=CARTESIAN_POINT('Ctrl Pts',(144.729707021216,21.4999999999999,2.03896089378841));
#9877=CARTESIAN_POINT('Ctrl Pts',(144.758777673282,21.4955937057347,2.04285168076792));
#9878=CARTESIAN_POINT('Ctrl Pts',(144.817440852233,21.4779567710066,2.05836227087722));
#9879=CARTESIAN_POINT('Ctrl Pts',(144.845615509175,21.4640057619501,2.07060652861162));
#9880=CARTESIAN_POINT('Ctrl Pts',(144.902101216584,21.4250399915451,2.10457296342855));
#9881=CARTESIAN_POINT('Ctrl Pts',(144.927927434013,21.3982203268002,2.12780612534895));
#9882=CARTESIAN_POINT('Ctrl Pts',(144.964853191741,21.3441129754836,2.17419410934394));
#9883=CARTESIAN_POINT('Ctrl Pts',(144.977648024164,21.3172521646773,2.19704892779082));
#9884=CARTESIAN_POINT('Ctrl Pts',(144.995183002517,21.2612564013421,2.24427435401479));
#9885=CARTESIAN_POINT('Ctrl Pts',(144.99975020409,21.2318642099517,2.26885093208373));
#9886=CARTESIAN_POINT('Ctrl Pts',(144.999996676586,21.2016304842259,2.29390907945453));
#9887=CARTESIAN_POINT('Ctrl Pts',(145.,21.2008152808565,2.29458456963201));
#9888=CARTESIAN_POINT('Ctrl Pts',(145.,21.1999999999999,2.29525996204705));
#9889=CARTESIAN_POINT('',(144.7,21.4999999999999,1.01948044689421));
#9890=CARTESIAN_POINT('Origin',(141.,-21.1999999999999,15.7));
#9891=CARTESIAN_POINT('',(141.,-21.4999999999999,15.7));
#9892=CARTESIAN_POINT('',(141.,-21.1999999999999,16.));
#9893=CARTESIAN_POINT('Origin',(129.3,-21.1999999999999,1.01948044689421));
#9894=CARTESIAN_POINT('',(129.,-21.1999999999999,2.29525996204705));
#9895=CARTESIAN_POINT('',(129.,-21.1999999999999,1.01948044689421));
#9896=CARTESIAN_POINT('',(129.3,-21.4999999999999,2.03896089378841));
#9897=CARTESIAN_POINT('Ctrl Pts',(129.3,-21.4999999999999,2.03896089378841));
#9898=CARTESIAN_POINT('Ctrl Pts',(129.270292978784,-21.4999999999999,2.03896089378841));
#9899=CARTESIAN_POINT('Ctrl Pts',(129.241222326718,-21.4955937057347,2.04285168076791));
#9900=CARTESIAN_POINT('Ctrl Pts',(129.182559147767,-21.4779567710066,2.05836227087723));
#9901=CARTESIAN_POINT('Ctrl Pts',(129.154384490824,-21.4640057619501,2.07060652861162));
#9902=CARTESIAN_POINT('Ctrl Pts',(129.097898783416,-21.4250399915451,2.10457296342855));
#9903=CARTESIAN_POINT('Ctrl Pts',(129.072072565987,-21.3982203268002,2.12780612534895));
#9904=CARTESIAN_POINT('Ctrl Pts',(129.035146808259,-21.3441129754836,2.17419410934393));
#9905=CARTESIAN_POINT('Ctrl Pts',(129.022351975836,-21.3172521646773,2.19704892779082));
#9906=CARTESIAN_POINT('Ctrl Pts',(129.004816997483,-21.2612564013421,2.24427435401479));
#9907=CARTESIAN_POINT('Ctrl Pts',(129.000249795909,-21.2318642099517,2.26885093208373));
#9908=CARTESIAN_POINT('Ctrl Pts',(129.000003323414,-21.2016304842259,2.29390907945453));
#9909=CARTESIAN_POINT('Ctrl Pts',(129.,-21.2008152808565,2.29458456963201));
#9910=CARTESIAN_POINT('Ctrl Pts',(129.,-21.1999999999999,2.29525996204705));
#9911=CARTESIAN_POINT('',(129.3,-21.4999999999999,1.01948044689421));
#9912=CARTESIAN_POINT('Origin',(129.3,21.9999999999999,-1.92966607280848));
#9913=CARTESIAN_POINT('Origin',(129.3,21.9999999999999,-1.92966607280848));
#9914=CARTESIAN_POINT('Origin',(129.,21.9999999999999,-1.92966607280848));
#9915=CARTESIAN_POINT('Origin',(144.7,-21.1999999999999,1.01948044689421));
#9916=CARTESIAN_POINT('',(144.7,-21.4999999999999,2.03896089378841));
#9917=CARTESIAN_POINT('',(144.7,-21.4999999999999,1.01948044689421));
#9918=CARTESIAN_POINT('',(145.,-21.1999999999999,2.29525996204705));
#9919=CARTESIAN_POINT('Ctrl Pts',(145.,-21.1999999999999,2.29525996204705));
#9920=CARTESIAN_POINT('Ctrl Pts',(145.,-21.2008152808404,2.29458456964534));
#9921=CARTESIAN_POINT('Ctrl Pts',(144.999996676585,-21.2016304842412,2.29390907943587));
#9922=CARTESIAN_POINT('Ctrl Pts',(144.999750204092,-21.2318642097648,2.26885093228761));
#9923=CARTESIAN_POINT('Ctrl Pts',(144.995183002528,-21.2612564013074,2.24427435404393));
#9924=CARTESIAN_POINT('Ctrl Pts',(144.977648024164,-21.3172521646786,2.19704892778962));
#9925=CARTESIAN_POINT('Ctrl Pts',(144.964853191741,-21.3441129754842,2.17419410934337));
#9926=CARTESIAN_POINT('Ctrl Pts',(144.927927434013,-21.3982203268002,2.12780612534895));
#9927=CARTESIAN_POINT('Ctrl Pts',(144.902101216584,-21.4250399915451,2.10457296342854));
#9928=CARTESIAN_POINT('Ctrl Pts',(144.845615509175,-21.4640057619501,2.07060652861161));
#9929=CARTESIAN_POINT('Ctrl Pts',(144.817440852233,-21.4779567710066,2.05836227087722));
#9930=CARTESIAN_POINT('Ctrl Pts',(144.758777673282,-21.4955937057347,2.04285168076792));
#9931=CARTESIAN_POINT('Ctrl Pts',(144.729707021216,-21.4999999999999,2.03896089378841));
#9932=CARTESIAN_POINT('Ctrl Pts',(144.7,-21.4999999999999,2.03896089378841));
#9933=CARTESIAN_POINT('',(145.,-21.1999999999999,1.01948044689421));
#9934=CARTESIAN_POINT('Origin',(144.7,21.9999999999999,-1.92966607280848));
#9935=CARTESIAN_POINT('Origin',(145.,21.9999999999999,-1.92966607280848));
#9936=CARTESIAN_POINT('Origin',(144.7,21.9999999999999,-1.92966607280848));
#9937=CARTESIAN_POINT('Origin',(129.3,-21.9999999999999,-1.92966607280848));
#9938=CARTESIAN_POINT('Origin',(129.,-21.9999999999999,-1.92966607280848));
#9939=CARTESIAN_POINT('Origin',(129.3,-21.9999999999999,-1.92966607280848));
#9940=CARTESIAN_POINT('Origin',(144.7,-21.9999999999999,-1.92966607280848));
#9941=CARTESIAN_POINT('Origin',(144.7,-21.9999999999999,-1.92966607280848));
#9942=CARTESIAN_POINT('Origin',(145.,-21.9999999999999,-1.92966607280848));
#9943=CARTESIAN_POINT('Origin',(144.7,15.,15.7));
#9944=CARTESIAN_POINT('',(145.,15.,15.7));
#9945=CARTESIAN_POINT('',(144.7,15.,16.));
#9946=CARTESIAN_POINT('Origin',(141.,-22.7999999999999,15.7));
#9947=CARTESIAN_POINT('',(141.,-22.4999999999999,15.7));
#9948=CARTESIAN_POINT('',(141.,-22.7999999999999,16.));
#9949=CARTESIAN_POINT('Origin',(129.3,-15.,15.7));
#9950=CARTESIAN_POINT('',(129.,-15.,15.7));
#9951=CARTESIAN_POINT('',(129.3,-15.,16.));
#9952=CARTESIAN_POINT('Origin',(141.,-29.7,15.7));
#9953=CARTESIAN_POINT('',(141.,-30.,15.7));
#9954=CARTESIAN_POINT('',(141.,-29.7,16.));
#9955=CARTESIAN_POINT('Origin',(129.3,2.5,-10.3));
#9956=CARTESIAN_POINT('',(129.,2.5,-10.3));
#9957=CARTESIAN_POINT('Origin',(133.,30.3,-9.7));
#9958=CARTESIAN_POINT('',(133.,30.,-9.7));
#9959=CARTESIAN_POINT('Origin',(144.7,32.5,-10.3));
#9960=CARTESIAN_POINT('',(145.,32.5,-10.3));
#9961=CARTESIAN_POINT('Origin',(141.,-30.3,-9.7));
#9962=CARTESIAN_POINT('',(141.,-30.,-9.7));
#9963=CARTESIAN_POINT('Origin',(129.3,-32.5,-10.3));
#9964=CARTESIAN_POINT('',(129.,-32.5,-10.3));
#9965=CARTESIAN_POINT('Origin',(129.3,39.7,-8.));
#9966=CARTESIAN_POINT('',(129.3,40.,-8.));
#9967=CARTESIAN_POINT('',(129.,39.7,-8.));
#9968=CARTESIAN_POINT('Origin',(144.7,-2.5,-10.3));
#9969=CARTESIAN_POINT('',(145.,-2.5,-10.3));
#9970=CARTESIAN_POINT('Origin',(144.7,39.7,-8.));
#9971=CARTESIAN_POINT('',(145.,39.7,-8.));
#9972=CARTESIAN_POINT('',(144.7,40.,-8.));
#9973=CARTESIAN_POINT('Origin',(141.,-39.7,-10.3));
#9974=CARTESIAN_POINT('',(141.,-40.,-10.3));
#9975=CARTESIAN_POINT('Origin',(141.,-39.7,-15.7));
#9976=CARTESIAN_POINT('',(141.,-40.,-15.7));
#9977=CARTESIAN_POINT('',(141.,-39.7,-16.));
#9978=CARTESIAN_POINT('Origin',(145.,21.4999999999999,2.03896089378841));
#9979=CARTESIAN_POINT('',(145.,21.4999999999999,2.03896089378841));
#9980=CARTESIAN_POINT('Origin',(145.,21.9999999999999,-1.92966607280848));
#9981=CARTESIAN_POINT('',(145.,22.4999999999999,2.03896089378841));
#9982=CARTESIAN_POINT('Origin',(145.,-21.9999999999999,-1.92966607280848));
#9983=CARTESIAN_POINT('',(145.,-22.4999999999999,2.03896089378841));
#9984=CARTESIAN_POINT('',(145.,-21.4999999999999,2.03896089378841));
#9985=CARTESIAN_POINT('Origin',(145.,-21.4999999999999,2.03896089378841));
#9986=CARTESIAN_POINT('Origin',(137.,-4.44089209850063E-15,-16.));
#9987=CARTESIAN_POINT('Origin',(145.,-40.,-16.));
#9988=CARTESIAN_POINT('Origin',(145.,40.,-16.));
#9989=CARTESIAN_POINT('Origin',(145.,-30.,0.));
#9990=CARTESIAN_POINT('Origin',(137.,-4.44089209850063E-15,16.));
#9991=CARTESIAN_POINT('Origin',(129.,30.,0.));
#9992=CARTESIAN_POINT('Origin',(137.,-4.44089209850063E-15,16.));
#9993=CARTESIAN_POINT('Origin',(145.,30.,0.));
#9994=CARTESIAN_POINT('Origin',(137.,-4.44089209850063E-15,16.));
#9995=CARTESIAN_POINT('Origin',(129.,-30.,0.));
#9996=CARTESIAN_POINT('Origin',(145.,22.4999999999999,16.));
#9997=CARTESIAN_POINT('Origin',(145.,-22.4999999999999,16.));
#9998=CARTESIAN_POINT('',(0.,0.,0.));
#9999=CARTESIAN_POINT('Origin',(129.,0.,0.));
#10000=CARTESIAN_POINT('',(129.,4.925,6.03138548580071E-16));
#10001=CARTESIAN_POINT('Origin',(129.,0.,0.));
#10002=CARTESIAN_POINT('Origin',(-125.,0.,0.));
#10003=CARTESIAN_POINT('',(-129.,4.925,6.03138548580071E-16));
#10004=CARTESIAN_POINT('Origin',(-129.,0.,0.));
#10005=CARTESIAN_POINT('',(-125.,4.925,-6.03138548580071E-16));
#10006=CARTESIAN_POINT('Origin',(-129.,0.,0.));
#10007=CARTESIAN_POINT('',(0.,0.,0.));
#10008=CARTESIAN_POINT('Origin',(13.3,21.9999999999999,-1.92966607280848));
#10009=CARTESIAN_POINT('',(13.,21.9999999999999,-6.22966607280848));
#10010=CARTESIAN_POINT('Origin',(13.,21.9999999999999,-1.92966607280848));
#10011=CARTESIAN_POINT('',(13.3,21.9999999999999,-5.92966607280848));
#10012=CARTESIAN_POINT('Origin',(13.3,21.9999999999999,-6.22966607280848));
#10013=CARTESIAN_POINT('',(13.3,25.9999999999999,-1.92966607280848));
#10014=CARTESIAN_POINT('Origin',(13.3,21.9999999999999,-1.92966607280848));
#10015=CARTESIAN_POINT('Origin',(13.3,21.9999999999999,-1.92966607280848));
#10016=CARTESIAN_POINT('Origin',(13.,21.9999999999999,-1.92966607280848));
#10017=CARTESIAN_POINT('',(13.,21.9999999999999,2.77033392719152));
#10018=CARTESIAN_POINT('Origin',(13.,21.9999999999999,-1.92966607280848));
#10019=CARTESIAN_POINT('Origin',(29.,21.9999999999999,-1.92966607280848));
#10020=CARTESIAN_POINT('',(28.7,25.9999999999999,-1.92966607280848));
#10021=CARTESIAN_POINT('',(29.,25.9999999999999,-1.92966607280848));
#10022=CARTESIAN_POINT('',(28.7,21.9999999999999,2.07033392719152));
#10023=CARTESIAN_POINT('Origin',(28.7,21.9999999999999,-1.92966607280848));
#10024=CARTESIAN_POINT('Origin',(28.7,21.9999999999999,-1.92966607280848));
#10025=CARTESIAN_POINT('Origin',(13.3,21.9999999999999,-1.92966607280848));
#10026=CARTESIAN_POINT('',(13.3,21.9999999999999,3.07033392719152));
#10027=CARTESIAN_POINT('Origin',(13.3,21.9999999999999,2.77033392719152));
#10028=CARTESIAN_POINT('',(13.3,26.9999999999999,-1.92966607280848));
#10029=CARTESIAN_POINT('Origin',(13.3,21.9999999999999,-1.92966607280848));
#10030=CARTESIAN_POINT('Origin',(13.3,21.9999999999999,-1.92966607280848));
#10031=CARTESIAN_POINT('Origin',(29.,21.9999999999999,-1.92966607280848));
#10032=CARTESIAN_POINT('',(28.7,26.9999999999999,-1.92966607280848));
#10033=CARTESIAN_POINT('',(29.,26.9999999999999,-1.92966607280848));
#10034=CARTESIAN_POINT('',(28.7,21.9999999999999,-6.92966607280848));
#10035=CARTESIAN_POINT('Origin',(28.7,21.9999999999999,-1.92966607280848));
#10036=CARTESIAN_POINT('Origin',(28.7,21.9999999999999,-1.92966607280848));
#10037=CARTESIAN_POINT('Origin',(28.7,21.9999999999999,-1.92966607280848));
#10038=CARTESIAN_POINT('',(29.,21.9999999999999,2.37033392719152));
#10039=CARTESIAN_POINT('Origin',(29.,21.9999999999999,-1.92966607280848));
#10040=CARTESIAN_POINT('Origin',(28.7,21.9999999999999,2.37033392719152));
#10041=CARTESIAN_POINT('Origin',(29.,21.9999999999999,-1.92966607280848));
#10042=CARTESIAN_POINT('',(29.,21.9999999999999,-6.62966607280848));
#10043=CARTESIAN_POINT('Origin',(29.,21.9999999999999,-1.92966607280848));
#10044=CARTESIAN_POINT('Origin',(28.7,21.9999999999999,-1.92966607280848));
#10045=CARTESIAN_POINT('Origin',(28.7,21.9999999999999,-6.62966607280848));
#10046=CARTESIAN_POINT('',(0.,0.,0.));
#10047=CARTESIAN_POINT('Origin',(-145.,21.9999999999999,-1.92966607280848));
#10048=CARTESIAN_POINT('',(-145.,17.9999999999999,-1.92966607280848));
#10049=CARTESIAN_POINT('Origin',(-145.,21.9999999999999,-1.92966607280848));
#10050=CARTESIAN_POINT('Origin',(-125.,21.9999999999999,-1.92966607280848));
#10051=CARTESIAN_POINT('',(145.,17.9999999999999,-1.92966607280848));
#10052=CARTESIAN_POINT('Origin',(145.,21.9999999999999,-1.92966607280848));
#10053=CARTESIAN_POINT('',(-125.,17.9999999999999,-1.92966607280848));
#10054=CARTESIAN_POINT('Origin',(145.,21.9999999999999,-1.92966607280848));
#10055=CARTESIAN_POINT('',(0.,0.,0.));
#10056=CARTESIAN_POINT('Origin',(-145.,-21.9999999999999,-1.92966607280848));
#10057=CARTESIAN_POINT('',(-145.,-17.9999999999999,-1.92966607280848));
#10058=CARTESIAN_POINT('Origin',(-145.,-21.9999999999999,-1.92966607280848));
#10059=CARTESIAN_POINT('Origin',(-125.,-21.9999999999999,-1.92966607280848));
#10060=CARTESIAN_POINT('',(145.,-17.9999999999999,-1.92966607280848));
#10061=CARTESIAN_POINT('Origin',(145.,-21.9999999999999,-1.92966607280848));
#10062=CARTESIAN_POINT('',(-125.,-17.9999999999999,-1.92966607280848));
#10063=CARTESIAN_POINT('Origin',(145.,-21.9999999999999,-1.92966607280848));
#10064=CARTESIAN_POINT('',(0.,0.,0.));
#10065=CARTESIAN_POINT('Origin',(-13.3,21.9999999999999,-1.92966607280848));
#10066=CARTESIAN_POINT('',(-13.,21.9999999999999,-6.22966607280848));
#10067=CARTESIAN_POINT('Origin',(-13.,21.9999999999999,-1.92966607280848));
#10068=CARTESIAN_POINT('',(-13.3,21.9999999999999,-5.92966607280848));
#10069=CARTESIAN_POINT('Origin',(-13.3,21.9999999999999,-6.22966607280848));
#10070=CARTESIAN_POINT('',(-13.3,25.9999999999999,-1.92966607280848));
#10071=CARTESIAN_POINT('Origin',(-13.3,21.9999999999999,-1.92966607280848));
#10072=CARTESIAN_POINT('Origin',(-13.3,21.9999999999999,-1.92966607280848));
#10073=CARTESIAN_POINT('Origin',(-13.,21.9999999999999,-1.92966607280848));
#10074=CARTESIAN_POINT('',(-13.,21.9999999999999,2.77033392719152));
#10075=CARTESIAN_POINT('Origin',(-13.,21.9999999999999,-1.92966607280848));
#10076=CARTESIAN_POINT('Origin',(-29.,21.9999999999999,-1.92966607280848));
#10077=CARTESIAN_POINT('',(-28.7,25.9999999999999,-1.92966607280848));
#10078=CARTESIAN_POINT('',(-29.,25.9999999999999,-1.92966607280848));
#10079=CARTESIAN_POINT('',(-28.7,21.9999999999999,2.07033392719152));
#10080=CARTESIAN_POINT('Origin',(-28.7,21.9999999999999,-1.92966607280848));
#10081=CARTESIAN_POINT('Origin',(-28.7,21.9999999999999,-1.92966607280848));
#10082=CARTESIAN_POINT('Origin',(-13.3,21.9999999999999,-1.92966607280848));
#10083=CARTESIAN_POINT('',(-13.3,21.9999999999999,3.07033392719152));
#10084=CARTESIAN_POINT('Origin',(-13.3,21.9999999999999,2.77033392719152));
#10085=CARTESIAN_POINT('',(-13.3,26.9999999999999,-1.92966607280848));
#10086=CARTESIAN_POINT('Origin',(-13.3,21.9999999999999,-1.92966607280848));
#10087=CARTESIAN_POINT('Origin',(-13.3,21.9999999999999,-1.92966607280848));
#10088=CARTESIAN_POINT('Origin',(-29.,21.9999999999999,-1.92966607280848));
#10089=CARTESIAN_POINT('',(-28.7,26.9999999999999,-1.92966607280848));
#10090=CARTESIAN_POINT('',(-29.,26.9999999999999,-1.92966607280848));
#10091=CARTESIAN_POINT('',(-28.7,21.9999999999999,-6.92966607280848));
#10092=CARTESIAN_POINT('Origin',(-28.7,21.9999999999999,-1.92966607280848));
#10093=CARTESIAN_POINT('Origin',(-28.7,21.9999999999999,-1.92966607280848));
#10094=CARTESIAN_POINT('Origin',(-28.7,21.9999999999999,-1.92966607280848));
#10095=CARTESIAN_POINT('',(-29.,21.9999999999999,2.37033392719152));
#10096=CARTESIAN_POINT('Origin',(-29.,21.9999999999999,-1.92966607280848));
#10097=CARTESIAN_POINT('Origin',(-28.7,21.9999999999999,2.37033392719152));
#10098=CARTESIAN_POINT('Origin',(-29.,21.9999999999999,-1.92966607280848));
#10099=CARTESIAN_POINT('',(-29.,21.9999999999999,-6.62966607280848));
#10100=CARTESIAN_POINT('Origin',(-29.,21.9999999999999,-1.92966607280848));
#10101=CARTESIAN_POINT('Origin',(-28.7,21.9999999999999,-1.92966607280848));
#10102=CARTESIAN_POINT('Origin',(-28.7,21.9999999999999,-6.62966607280848));
#10103=CARTESIAN_POINT('',(0.,0.,0.));
#10104=CARTESIAN_POINT('Origin',(-133.037195913696,35.,-10.3));
#10105=CARTESIAN_POINT('',(-135.037195913696,35.,-10.3));
#10106=CARTESIAN_POINT('Origin',(-133.037195913696,35.,-10.3));
#10107=CARTESIAN_POINT('',(-135.337195913696,35.,-10.));
#10108=CARTESIAN_POINT('Origin',(-135.337195913696,35.,-10.3));
#10109=CARTESIAN_POINT('Origin',(-133.037195913696,35.,-10.));
#10110=CARTESIAN_POINT('Origin',(-137.,35.,-10.));
#10111=CARTESIAN_POINT('',(-144.7,39.7,-10.));
#10112=CARTESIAN_POINT('',(-129.3,39.7,-10.));
#10113=CARTESIAN_POINT('',(-141.,39.7,-10.));
#10114=CARTESIAN_POINT('',(-144.7,30.3,-10.));
#10115=CARTESIAN_POINT('',(-144.7,32.5,-10.));
#10116=CARTESIAN_POINT('',(-129.3,30.3,-10.));
#10117=CARTESIAN_POINT('',(-133.,30.3,-10.));
#10118=CARTESIAN_POINT('',(-129.3,2.5,-10.));
#10119=CARTESIAN_POINT('',(-143.262804086304,35.,-10.));
#10120=CARTESIAN_POINT('Origin',(-140.962804086304,35.,-10.));
#10121=CARTESIAN_POINT('Origin',(-133.037195913696,35.,-16.));
#10122=CARTESIAN_POINT('',(-135.037195913696,35.,-16.));
#10123=CARTESIAN_POINT('',(-135.037195913696,35.,-16.));
#10124=CARTESIAN_POINT('Origin',(-133.037195913696,35.,-16.));
#10125=CARTESIAN_POINT('Origin',(-140.962804086304,35.,-10.3));
#10126=CARTESIAN_POINT('',(-142.962804086304,35.,-10.3));
#10127=CARTESIAN_POINT('Origin',(-140.962804086304,35.,-10.3));
#10128=CARTESIAN_POINT('Origin',(-143.262804086304,35.,-10.3));
#10129=CARTESIAN_POINT('Origin',(-140.962804086304,35.,-16.));
#10130=CARTESIAN_POINT('',(-142.962804086304,35.,-16.));
#10131=CARTESIAN_POINT('',(-142.962804086304,35.,-16.));
#10132=CARTESIAN_POINT('Origin',(-140.962804086304,35.,-16.));
#10133=CARTESIAN_POINT('Origin',(-133.037195913696,-35.,-10.3));
#10134=CARTESIAN_POINT('',(-130.737195913696,-35.,-10.));
#10135=CARTESIAN_POINT('Origin',(-133.037195913696,-35.,-10.));
#10136=CARTESIAN_POINT('',(-131.037195913696,-35.,-10.3));
#10137=CARTESIAN_POINT('Origin',(-130.737195913696,-35.,-10.3));
#10138=CARTESIAN_POINT('',(-135.037195913696,-35.,-10.3));
#10139=CARTESIAN_POINT('Origin',(-133.037195913696,-35.,-10.3));
#10140=CARTESIAN_POINT('Origin',(-133.037195913696,-35.,-10.3));
#10141=CARTESIAN_POINT('Origin',(-137.,-35.,-10.));
#10142=CARTESIAN_POINT('',(-144.7,-30.3,-10.));
#10143=CARTESIAN_POINT('',(-129.3,-30.3,-10.));
#10144=CARTESIAN_POINT('',(-141.,-30.3,-10.));
#10145=CARTESIAN_POINT('',(-144.7,-39.7,-10.));
#10146=CARTESIAN_POINT('',(-144.7,-2.5,-10.));
#10147=CARTESIAN_POINT('',(-129.3,-39.7,-10.));
#10148=CARTESIAN_POINT('',(-141.,-39.7,-10.));
#10149=CARTESIAN_POINT('',(-129.3,-32.5,-10.));
#10150=CARTESIAN_POINT('',(-138.662804086304,-35.,-10.));
#10151=CARTESIAN_POINT('Origin',(-140.962804086304,-35.,-10.));
#10152=CARTESIAN_POINT('Origin',(-133.037195913696,-35.,-16.));
#10153=CARTESIAN_POINT('',(-135.037195913696,-35.,-16.));
#10154=CARTESIAN_POINT('',(-135.037195913696,-35.,-16.));
#10155=CARTESIAN_POINT('Origin',(-133.037195913696,-35.,-16.));
#10156=CARTESIAN_POINT('Origin',(-140.962804086304,-35.,-10.3));
#10157=CARTESIAN_POINT('',(-138.962804086304,-35.,-10.3));
#10158=CARTESIAN_POINT('Origin',(-138.662804086304,-35.,-10.3));
#10159=CARTESIAN_POINT('',(-142.962804086304,-35.,-10.3));
#10160=CARTESIAN_POINT('Origin',(-140.962804086304,-35.,-10.3));
#10161=CARTESIAN_POINT('Origin',(-140.962804086304,-35.,-10.3));
#10162=CARTESIAN_POINT('Origin',(-140.962804086304,-35.,-16.));
#10163=CARTESIAN_POINT('',(-142.962804086304,-35.,-16.));
#10164=CARTESIAN_POINT('',(-142.962804086304,-35.,-16.));
#10165=CARTESIAN_POINT('Origin',(-140.962804086304,-35.,-16.));
#10166=CARTESIAN_POINT('Origin',(-144.7,-39.7,-15.7));
#10167=CARTESIAN_POINT('',(-145.,-39.7,-15.7));
#10168=CARTESIAN_POINT('',(-144.7,-40.,-15.7));
#10169=CARTESIAN_POINT('Origin',(-144.7,-39.7,-15.7));
#10170=CARTESIAN_POINT('',(-144.7,-39.7,-16.));
#10171=CARTESIAN_POINT('Origin',(-144.7,-39.7,-15.7));
#10172=CARTESIAN_POINT('Origin',(-144.7,-39.7,-15.7));
#10173=CARTESIAN_POINT('Origin',(-129.3,-39.7,-15.7));
#10174=CARTESIAN_POINT('',(-129.3,-39.7,-16.));
#10175=CARTESIAN_POINT('',(-129.3,-40.,-15.7));
#10176=CARTESIAN_POINT('Origin',(-129.3,-39.7,-15.7));
#10177=CARTESIAN_POINT('',(-129.,-39.7,-15.7));
#10178=CARTESIAN_POINT('Origin',(-129.3,-39.7,-15.7));
#10179=CARTESIAN_POINT('Origin',(-129.3,-39.7,-15.7));
#10180=CARTESIAN_POINT('Origin',(-144.7,39.7,-15.7));
#10181=CARTESIAN_POINT('',(-144.7,39.7,-16.));
#10182=CARTESIAN_POINT('',(-144.7,40.,-15.7));
#10183=CARTESIAN_POINT('Origin',(-144.7,39.7,-15.7));
#10184=CARTESIAN_POINT('',(-145.,39.7,-15.7));
#10185=CARTESIAN_POINT('Origin',(-144.7,39.7,-15.7));
#10186=CARTESIAN_POINT('Origin',(-144.7,39.7,-15.7));
#10187=CARTESIAN_POINT('Origin',(-144.7,15.,-15.7));
#10188=CARTESIAN_POINT('',(-144.7,15.,-16.));
#10189=CARTESIAN_POINT('',(-145.,15.,-15.7));
#10190=CARTESIAN_POINT('Origin',(-144.7,-39.7,-10.3));
#10191=CARTESIAN_POINT('',(-145.,-39.7,-10.3));
#10192=CARTESIAN_POINT('Origin',(-144.7,-39.7,-10.3));
#10193=CARTESIAN_POINT('',(-144.7,-40.,-10.3));
#10194=CARTESIAN_POINT('Origin',(-144.7,-39.7,-10.3));
#10195=CARTESIAN_POINT('Origin',(-144.7,-39.7,-10.3));
#10196=CARTESIAN_POINT('Origin',(-144.7,-39.7,-8.));
#10197=CARTESIAN_POINT('',(-145.,-39.7,-8.));
#10198=CARTESIAN_POINT('',(-144.7,-40.,-8.));
#10199=CARTESIAN_POINT('Origin',(-129.3,39.7,-15.7));
#10200=CARTESIAN_POINT('',(-129.,39.7,-15.7));
#10201=CARTESIAN_POINT('',(-129.3,40.,-15.7));
#10202=CARTESIAN_POINT('Origin',(-129.3,39.7,-15.7));
#10203=CARTESIAN_POINT('',(-129.3,39.7,-16.));
#10204=CARTESIAN_POINT('Origin',(-129.3,39.7,-15.7));
#10205=CARTESIAN_POINT('Origin',(-129.3,39.7,-15.7));
#10206=CARTESIAN_POINT('Origin',(-129.3,-15.,-15.7));
#10207=CARTESIAN_POINT('',(-129.,-15.,-15.7));
#10208=CARTESIAN_POINT('',(-129.3,-15.,-16.));
#10209=CARTESIAN_POINT('Origin',(-141.,39.7,-15.7));
#10210=CARTESIAN_POINT('',(-141.,40.,-15.7));
#10211=CARTESIAN_POINT('',(-141.,39.7,-16.));
#10212=CARTESIAN_POINT('Origin',(-129.3,-39.7,-10.3));
#10213=CARTESIAN_POINT('',(-129.3,-40.,-10.3));
#10214=CARTESIAN_POINT('Origin',(-129.3,-39.7,-10.3));
#10215=CARTESIAN_POINT('',(-129.,-39.7,-10.3));
#10216=CARTESIAN_POINT('Origin',(-129.3,-39.7,-10.3));
#10217=CARTESIAN_POINT('Origin',(-129.3,-39.7,-10.3));
#10218=CARTESIAN_POINT('Origin',(-129.3,-39.7,-8.));
#10219=CARTESIAN_POINT('',(-129.3,-40.,-8.));
#10220=CARTESIAN_POINT('',(-129.,-39.7,-8.));
#10221=CARTESIAN_POINT('Origin',(-144.7,39.7,-10.3));
#10222=CARTESIAN_POINT('',(-145.,39.7,-10.3));
#10223=CARTESIAN_POINT('',(-144.7,40.,-10.3));
#10224=CARTESIAN_POINT('Origin',(-144.7,39.7,-10.3));
#10225=CARTESIAN_POINT('Origin',(-144.7,39.7,-10.3));
#10226=CARTESIAN_POINT('Origin',(-144.7,39.7,-10.3));
#10227=CARTESIAN_POINT('Origin',(-144.7,-30.3,-9.7));
#10228=CARTESIAN_POINT('',(-144.7,-30.,-9.7));
#10229=CARTESIAN_POINT('Origin',(-144.7,-30.3,-9.7));
#10230=CARTESIAN_POINT('',(-145.,-29.7,-9.7));
#10231=CARTESIAN_POINT('Origin',(-144.7,-29.7,-9.7));
#10232=CARTESIAN_POINT('',(-145.,-30.3,-10.3));
#10233=CARTESIAN_POINT('Origin',(-145.,-30.3,-9.7));
#10234=CARTESIAN_POINT('Origin',(-144.7,-30.3,-10.3));
#10235=CARTESIAN_POINT('Origin',(-129.3,39.7,-10.3));
#10236=CARTESIAN_POINT('',(-129.3,40.,-10.3));
#10237=CARTESIAN_POINT('',(-129.,39.7,-10.3));
#10238=CARTESIAN_POINT('Origin',(-129.3,39.7,-10.3));
#10239=CARTESIAN_POINT('Origin',(-129.3,39.7,-10.3));
#10240=CARTESIAN_POINT('Origin',(-129.3,39.7,-10.3));
#10241=CARTESIAN_POINT('Origin',(-141.,39.7,-10.3));
#10242=CARTESIAN_POINT('',(-141.,40.,-10.3));
#10243=CARTESIAN_POINT('Origin',(-129.3,-30.3,-9.7));
#10244=CARTESIAN_POINT('',(-129.,-30.3,-10.3));
#10245=CARTESIAN_POINT('',(-129.,-29.7,-9.7));
#10246=CARTESIAN_POINT('Origin',(-129.,-30.3,-9.7));
#10247=CARTESIAN_POINT('',(-129.3,-30.,-9.7));
#10248=CARTESIAN_POINT('Origin',(-129.3,-29.7,-9.7));
#10249=CARTESIAN_POINT('Origin',(-129.3,-30.3,-9.7));
#10250=CARTESIAN_POINT('Origin',(-129.3,-30.3,-10.3));
#10251=CARTESIAN_POINT('Origin',(-144.7,30.3,-9.7));
#10252=CARTESIAN_POINT('',(-145.,30.3,-10.3));
#10253=CARTESIAN_POINT('',(-145.,29.7,-9.7));
#10254=CARTESIAN_POINT('Origin',(-145.,30.3,-9.7));
#10255=CARTESIAN_POINT('',(-144.7,30.,-9.7));
#10256=CARTESIAN_POINT('Origin',(-144.7,29.7,-9.7));
#10257=CARTESIAN_POINT('Origin',(-144.7,30.3,-9.7));
#10258=CARTESIAN_POINT('Origin',(-144.7,30.3,-10.3));
#10259=CARTESIAN_POINT('Origin',(-144.7,-29.7,15.7));
#10260=CARTESIAN_POINT('',(-145.,-29.7,15.7));
#10261=CARTESIAN_POINT('',(-144.7,-29.7,16.));
#10262=CARTESIAN_POINT('Origin',(-144.7,-29.7,15.7));
#10263=CARTESIAN_POINT('',(-144.7,-30.,15.7));
#10264=CARTESIAN_POINT('Origin',(-144.7,-29.7,15.7));
#10265=CARTESIAN_POINT('Origin',(-144.7,-29.7,15.7));
#10266=CARTESIAN_POINT('Origin',(-144.7,-29.7,0.));
#10267=CARTESIAN_POINT('',(-144.7,-30.,0.));
#10268=CARTESIAN_POINT('',(-145.,-29.7,0.));
#10269=CARTESIAN_POINT('Origin',(-129.3,30.3,-9.7));
#10270=CARTESIAN_POINT('',(-129.3,30.,-9.7));
#10271=CARTESIAN_POINT('Origin',(-129.3,30.3,-9.7));
#10272=CARTESIAN_POINT('',(-129.,29.7,-9.7));
#10273=CARTESIAN_POINT('Origin',(-129.3,29.7,-9.7));
#10274=CARTESIAN_POINT('',(-129.,30.3,-10.3));
#10275=CARTESIAN_POINT('Origin',(-129.,30.3,-9.7));
#10276=CARTESIAN_POINT('Origin',(-129.3,30.3,-10.3));
#10277=CARTESIAN_POINT('Origin',(-129.3,-29.7,15.7));
#10278=CARTESIAN_POINT('',(-129.3,-30.,15.7));
#10279=CARTESIAN_POINT('',(-129.3,-29.7,16.));
#10280=CARTESIAN_POINT('Origin',(-129.3,-29.7,15.7));
#10281=CARTESIAN_POINT('',(-129.,-29.7,15.7));
#10282=CARTESIAN_POINT('Origin',(-129.3,-29.7,15.7));
#10283=CARTESIAN_POINT('Origin',(-129.3,-29.7,15.7));
#10284=CARTESIAN_POINT('Origin',(-129.3,-29.7,0.));
#10285=CARTESIAN_POINT('',(-129.3,-30.,0.));
#10286=CARTESIAN_POINT('',(-129.,-29.7,0.));
#10287=CARTESIAN_POINT('Origin',(-144.7,29.7,15.7));
#10288=CARTESIAN_POINT('',(-144.7,30.,15.7));
#10289=CARTESIAN_POINT('',(-144.7,29.7,16.));
#10290=CARTESIAN_POINT('Origin',(-144.7,29.7,15.7));
#10291=CARTESIAN_POINT('',(-145.,29.7,15.7));
#10292=CARTESIAN_POINT('Origin',(-144.7,29.7,15.7));
#10293=CARTESIAN_POINT('Origin',(-144.7,29.7,15.7));
#10294=CARTESIAN_POINT('Origin',(-144.7,29.7,0.));
#10295=CARTESIAN_POINT('',(-144.7,30.,0.));
#10296=CARTESIAN_POINT('',(-145.,29.7,0.));
#10297=CARTESIAN_POINT('Origin',(-144.7,-22.7999999999999,15.7));
#10298=CARTESIAN_POINT('',(-145.,-22.7999999999999,15.7));
#10299=CARTESIAN_POINT('',(-144.7,-22.4999999999999,15.7));
#10300=CARTESIAN_POINT('Origin',(-144.7,-22.7999999999999,15.7));
#10301=CARTESIAN_POINT('',(-144.7,-22.7999999999999,16.));
#10302=CARTESIAN_POINT('Origin',(-144.7,-22.7999999999999,15.7));
#10303=CARTESIAN_POINT('Origin',(-144.7,-22.7999999999999,15.7));
#10304=CARTESIAN_POINT('Origin',(-144.7,15.,15.7));
#10305=CARTESIAN_POINT('',(-144.7,15.,16.));
#10306=CARTESIAN_POINT('',(-145.,15.,15.7));
#10307=CARTESIAN_POINT('Origin',(-129.3,29.7,15.7));
#10308=CARTESIAN_POINT('',(-129.,29.7,15.7));
#10309=CARTESIAN_POINT('',(-129.3,29.7,16.));
#10310=CARTESIAN_POINT('Origin',(-129.3,29.7,15.7));
#10311=CARTESIAN_POINT('',(-129.3,30.,15.7));
#10312=CARTESIAN_POINT('Origin',(-129.3,29.7,15.7));
#10313=CARTESIAN_POINT('Origin',(-129.3,29.7,15.7));
#10314=CARTESIAN_POINT('Origin',(-129.3,29.7,0.));
#10315=CARTESIAN_POINT('',(-129.,29.7,0.));
#10316=CARTESIAN_POINT('',(-129.3,30.,0.));
#10317=CARTESIAN_POINT('Origin',(-133.,29.7,15.7));
#10318=CARTESIAN_POINT('',(-133.,29.7,16.));
#10319=CARTESIAN_POINT('',(-133.,30.,15.7));
#10320=CARTESIAN_POINT('Origin',(-129.3,-22.7999999999999,15.7));
#10321=CARTESIAN_POINT('',(-129.,-22.7999999999999,15.7));
#10322=CARTESIAN_POINT('',(-129.3,-22.7999999999999,16.));
#10323=CARTESIAN_POINT('Origin',(-129.3,-22.7999999999999,15.7));
#10324=CARTESIAN_POINT('',(-129.3,-22.4999999999999,15.7));
#10325=CARTESIAN_POINT('Origin',(-129.3,-22.7999999999999,15.7));
#10326=CARTESIAN_POINT('Origin',(-129.3,-22.7999999999999,15.7));
#10327=CARTESIAN_POINT('Origin',(-144.7,22.7999999999999,15.7));
#10328=CARTESIAN_POINT('',(-144.7,22.4999999999999,15.7));
#10329=CARTESIAN_POINT('',(-145.,22.7999999999999,15.7));
#10330=CARTESIAN_POINT('Origin',(-144.7,22.7999999999999,15.7));
#10331=CARTESIAN_POINT('',(-144.7,22.7999999999999,16.));
#10332=CARTESIAN_POINT('Origin',(-144.7,22.7999999999999,15.7));
#10333=CARTESIAN_POINT('Origin',(-144.7,22.7999999999999,15.7));
#10334=CARTESIAN_POINT('Origin',(-144.7,-22.7999999999999,8.));
#10335=CARTESIAN_POINT('',(-145.,-22.7999999999999,2.29525996204705));
#10336=CARTESIAN_POINT('',(-145.,-22.7999999999999,8.));
#10337=CARTESIAN_POINT('',(-144.7,-22.4999999999999,2.03896089378841));
#10338=CARTESIAN_POINT('',(-144.7,-22.4999999999999,8.));
#10339=CARTESIAN_POINT('Ctrl Pts',(-144.7,-22.4999999999999,2.03896089378841));
#10340=CARTESIAN_POINT('Ctrl Pts',(-144.729707021216,-22.4999999999999,
2.03896089378841));
#10341=CARTESIAN_POINT('Ctrl Pts',(-144.758777673282,-22.5044062942651,
2.04285168076791));
#10342=CARTESIAN_POINT('Ctrl Pts',(-144.817440852233,-22.5220432289933,
2.05836227087722));
#10343=CARTESIAN_POINT('Ctrl Pts',(-144.845615509175,-22.5359942380498,
2.07060652861162));
#10344=CARTESIAN_POINT('Ctrl Pts',(-144.902101216584,-22.5749600084548,
2.10457296342855));
#10345=CARTESIAN_POINT('Ctrl Pts',(-144.927927434013,-22.6017796731997,
2.12780612534896));
#10346=CARTESIAN_POINT('Ctrl Pts',(-144.964853191741,-22.6558870245156,
2.17419410934337));
#10347=CARTESIAN_POINT('Ctrl Pts',(-144.977648024164,-22.6827478353212,
2.19704892778962));
#10348=CARTESIAN_POINT('Ctrl Pts',(-144.995183002528,-22.7387435986925,
2.24427435404391));
#10349=CARTESIAN_POINT('Ctrl Pts',(-144.999750204092,-22.768135790235,2.26885093228759));
#10350=CARTESIAN_POINT('Ctrl Pts',(-144.999996676585,-22.7983695157586,
2.29390907943587));
#10351=CARTESIAN_POINT('Ctrl Pts',(-145.,-22.7991847191594,2.29458456964534));
#10352=CARTESIAN_POINT('Ctrl Pts',(-145.,-22.7999999999999,2.29525996204705));
#10353=CARTESIAN_POINT('Origin',(-129.3,22.7999999999999,15.7));
#10354=CARTESIAN_POINT('',(-129.,22.7999999999999,15.7));
#10355=CARTESIAN_POINT('',(-129.3,22.4999999999999,15.7));
#10356=CARTESIAN_POINT('Origin',(-129.3,22.7999999999999,15.7));
#10357=CARTESIAN_POINT('',(-129.3,22.7999999999999,16.));
#10358=CARTESIAN_POINT('Origin',(-129.3,22.7999999999999,15.7));
#10359=CARTESIAN_POINT('Origin',(-129.3,22.7999999999999,15.7));
#10360=CARTESIAN_POINT('Origin',(-129.3,-15.,15.7));
#10361=CARTESIAN_POINT('',(-129.3,-15.,16.));
#10362=CARTESIAN_POINT('',(-129.,-15.,15.7));
#10363=CARTESIAN_POINT('Origin',(-141.,22.7999999999999,15.7));
#10364=CARTESIAN_POINT('',(-141.,22.7999999999999,16.));
#10365=CARTESIAN_POINT('',(-141.,22.4999999999999,15.7));
#10366=CARTESIAN_POINT('Origin',(-129.3,-22.7999999999999,8.));
#10367=CARTESIAN_POINT('',(-129.3,-22.4999999999999,2.03896089378841));
#10368=CARTESIAN_POINT('',(-129.3,-22.4999999999999,8.));
#10369=CARTESIAN_POINT('',(-129.,-22.7999999999999,2.29525996204705));
#10370=CARTESIAN_POINT('',(-129.,-22.7999999999999,8.));
#10371=CARTESIAN_POINT('Ctrl Pts',(-129.,-22.7999999999999,2.29525996204705));
#10372=CARTESIAN_POINT('Ctrl Pts',(-129.,-22.7991847191433,2.29458456963201));
#10373=CARTESIAN_POINT('Ctrl Pts',(-129.000003323414,-22.798369515774,2.29390907945453));
#10374=CARTESIAN_POINT('Ctrl Pts',(-129.000249795909,-22.7681357900482,
2.26885093208373));
#10375=CARTESIAN_POINT('Ctrl Pts',(-129.004816997483,-22.7387435986578,
2.24427435401478));
#10376=CARTESIAN_POINT('Ctrl Pts',(-129.022351975836,-22.6827478353226,
2.19704892779083));
#10377=CARTESIAN_POINT('Ctrl Pts',(-129.035146808259,-22.6558870245162,
2.17419410934394));
#10378=CARTESIAN_POINT('Ctrl Pts',(-129.072072565987,-22.6017796731997,
2.12780612534895));
#10379=CARTESIAN_POINT('Ctrl Pts',(-129.097898783416,-22.5749600084547,
2.10457296342854));
#10380=CARTESIAN_POINT('Ctrl Pts',(-129.154384490824,-22.5359942380497,
2.07060652861162));
#10381=CARTESIAN_POINT('Ctrl Pts',(-129.182559147767,-22.5220432289933,
2.05836227087722));
#10382=CARTESIAN_POINT('Ctrl Pts',(-129.241222326718,-22.5044062942651,
2.04285168076791));
#10383=CARTESIAN_POINT('Ctrl Pts',(-129.270292978784,-22.4999999999999,
2.03896089378841));
#10384=CARTESIAN_POINT('Ctrl Pts',(-129.3,-22.4999999999999,2.03896089378841));
#10385=CARTESIAN_POINT('Origin',(-144.7,22.7999999999999,8.));
#10386=CARTESIAN_POINT('',(-144.7,22.4999999999999,2.03896089378841));
#10387=CARTESIAN_POINT('',(-144.7,22.4999999999999,8.));
#10388=CARTESIAN_POINT('',(-145.,22.7999999999999,2.29525996204705));
#10389=CARTESIAN_POINT('',(-145.,22.7999999999999,8.));
#10390=CARTESIAN_POINT('Ctrl Pts',(-145.,22.7999999999999,2.29525996204705));
#10391=CARTESIAN_POINT('Ctrl Pts',(-145.,22.7991847191433,2.29458456963199));
#10392=CARTESIAN_POINT('Ctrl Pts',(-144.999996676586,22.798369515774,2.29390907945454));
#10393=CARTESIAN_POINT('Ctrl Pts',(-144.99975020409,22.768135790048,2.26885093208354));
#10394=CARTESIAN_POINT('Ctrl Pts',(-144.995183002517,22.7387435986577,2.24427435401474));
#10395=CARTESIAN_POINT('Ctrl Pts',(-144.977648024164,22.6827478353226,2.19704892779082));
#10396=CARTESIAN_POINT('Ctrl Pts',(-144.964853191741,22.6558870245162,2.17419410934393));
#10397=CARTESIAN_POINT('Ctrl Pts',(-144.927927434013,22.6017796731997,2.12780612534896));
#10398=CARTESIAN_POINT('Ctrl Pts',(-144.902101216584,22.5749600084548,2.10457296342855));
#10399=CARTESIAN_POINT('Ctrl Pts',(-144.845615509175,22.5359942380498,2.07060652861164));
#10400=CARTESIAN_POINT('Ctrl Pts',(-144.817440852233,22.5220432289933,2.05836227087723));
#10401=CARTESIAN_POINT('Ctrl Pts',(-144.758777673282,22.5044062942651,2.04285168076791));
#10402=CARTESIAN_POINT('Ctrl Pts',(-144.729707021216,22.4999999999999,2.03896089378841));
#10403=CARTESIAN_POINT('Ctrl Pts',(-144.7,22.4999999999999,2.03896089378841));
#10404=CARTESIAN_POINT('Origin',(-129.3,22.7999999999999,8.));
#10405=CARTESIAN_POINT('',(-129.,22.7999999999999,2.29525996204705));
#10406=CARTESIAN_POINT('',(-129.,22.7999999999999,8.));
#10407=CARTESIAN_POINT('',(-129.3,22.4999999999999,2.03896089378841));
#10408=CARTESIAN_POINT('',(-129.3,22.4999999999999,8.));
#10409=CARTESIAN_POINT('Ctrl Pts',(-129.3,22.4999999999999,2.03896089378841));
#10410=CARTESIAN_POINT('Ctrl Pts',(-129.270292978784,22.4999999999999,2.03896089378841));
#10411=CARTESIAN_POINT('Ctrl Pts',(-129.241222326718,22.5044062942651,2.04285168076791));
#10412=CARTESIAN_POINT('Ctrl Pts',(-129.182559147767,22.5220432289932,2.05836227087722));
#10413=CARTESIAN_POINT('Ctrl Pts',(-129.154384490824,22.5359942380497,2.07060652861162));
#10414=CARTESIAN_POINT('Ctrl Pts',(-129.097898783416,22.5749600084547,2.10457296342855));
#10415=CARTESIAN_POINT('Ctrl Pts',(-129.072072565987,22.6017796731997,2.12780612534895));
#10416=CARTESIAN_POINT('Ctrl Pts',(-129.035146808259,22.6558870245162,2.17419410934394));
#10417=CARTESIAN_POINT('Ctrl Pts',(-129.022351975836,22.6827478353226,2.19704892779082));
#10418=CARTESIAN_POINT('Ctrl Pts',(-129.004816997483,22.7387435986577,2.24427435401479));
#10419=CARTESIAN_POINT('Ctrl Pts',(-129.000249795909,22.7681357900482,2.26885093208374));
#10420=CARTESIAN_POINT('Ctrl Pts',(-129.000003323414,22.798369515774,2.29390907945453));
#10421=CARTESIAN_POINT('Ctrl Pts',(-129.,22.7991847191433,2.29458456963201));
#10422=CARTESIAN_POINT('Ctrl Pts',(-129.,22.7999999999999,2.29525996204705));
#10423=CARTESIAN_POINT('Origin',(-144.7,-21.1999999999999,15.7));
#10424=CARTESIAN_POINT('',(-144.7,-21.4999999999999,15.7));
#10425=CARTESIAN_POINT('',(-145.,-21.1999999999999,15.7));
#10426=CARTESIAN_POINT('Origin',(-144.7,-21.1999999999999,15.7));
#10427=CARTESIAN_POINT('',(-144.7,-21.1999999999999,16.));
#10428=CARTESIAN_POINT('Origin',(-144.7,-21.1999999999999,15.7));
#10429=CARTESIAN_POINT('Origin',(-144.7,-21.1999999999999,15.7));
#10430=CARTESIAN_POINT('Origin',(-129.3,-21.1999999999999,15.7));
#10431=CARTESIAN_POINT('',(-129.,-21.1999999999999,15.7));
#10432=CARTESIAN_POINT('',(-129.3,-21.4999999999999,15.7));
#10433=CARTESIAN_POINT('Origin',(-129.3,-21.1999999999999,15.7));
#10434=CARTESIAN_POINT('',(-129.3,-21.1999999999999,16.));
#10435=CARTESIAN_POINT('Origin',(-129.3,-21.1999999999999,15.7));
#10436=CARTESIAN_POINT('Origin',(-129.3,-21.1999999999999,15.7));
#10437=CARTESIAN_POINT('Origin',(-144.7,21.1999999999999,15.7));
#10438=CARTESIAN_POINT('',(-145.,21.1999999999999,15.7));
#10439=CARTESIAN_POINT('',(-144.7,21.4999999999999,15.7));
#10440=CARTESIAN_POINT('Origin',(-144.7,21.1999999999999,15.7));
#10441=CARTESIAN_POINT('',(-144.7,21.1999999999999,16.));
#10442=CARTESIAN_POINT('Origin',(-144.7,21.1999999999999,15.7));
#10443=CARTESIAN_POINT('Origin',(-144.7,21.1999999999999,15.7));
#10444=CARTESIAN_POINT('Origin',(-144.7,15.,15.7));
#10445=CARTESIAN_POINT('',(-144.7,15.,16.));
#10446=CARTESIAN_POINT('',(-145.,15.,15.7));
#10447=CARTESIAN_POINT('Origin',(-129.3,21.1999999999999,15.7));
#10448=CARTESIAN_POINT('',(-129.,21.1999999999999,15.7));
#10449=CARTESIAN_POINT('',(-129.3,21.1999999999999,16.));
#10450=CARTESIAN_POINT('Origin',(-129.3,21.1999999999999,15.7));
#10451=CARTESIAN_POINT('',(-129.3,21.4999999999999,15.7));
#10452=CARTESIAN_POINT('Origin',(-129.3,21.1999999999999,15.7));
#10453=CARTESIAN_POINT('Origin',(-129.3,21.1999999999999,15.7));
#10454=CARTESIAN_POINT('Origin',(-129.3,21.1999999999999,1.01948044689421));
#10455=CARTESIAN_POINT('',(-129.3,21.4999999999999,2.03896089378841));
#10456=CARTESIAN_POINT('',(-129.3,21.4999999999999,1.01948044689421));
#10457=CARTESIAN_POINT('',(-129.,21.1999999999999,2.29525996204705));
#10458=CARTESIAN_POINT('',(-129.,21.1999999999999,1.01948044689421));
#10459=CARTESIAN_POINT('Ctrl Pts',(-129.,21.1999999999999,2.29525996204705));
#10460=CARTESIAN_POINT('Ctrl Pts',(-129.,21.2008152808565,2.29458456963201));
#10461=CARTESIAN_POINT('Ctrl Pts',(-129.000003323414,21.2016304842259,2.29390907945453));
#10462=CARTESIAN_POINT('Ctrl Pts',(-129.000249795909,21.2318642099517,2.26885093208371));
#10463=CARTESIAN_POINT('Ctrl Pts',(-129.004816997483,21.2612564013421,2.24427435401476));
#10464=CARTESIAN_POINT('Ctrl Pts',(-129.022351975836,21.3172521646773,2.19704892779083));
#10465=CARTESIAN_POINT('Ctrl Pts',(-129.035146808259,21.3441129754836,2.17419410934394));
#10466=CARTESIAN_POINT('Ctrl Pts',(-129.072072565987,21.3982203268002,2.12780612534896));
#10467=CARTESIAN_POINT('Ctrl Pts',(-129.097898783416,21.4250399915451,2.10457296342855));
#10468=CARTESIAN_POINT('Ctrl Pts',(-129.154384490824,21.4640057619501,2.07060652861162));
#10469=CARTESIAN_POINT('Ctrl Pts',(-129.182559147767,21.4779567710066,2.05836227087723));
#10470=CARTESIAN_POINT('Ctrl Pts',(-129.241222326718,21.4955937057348,2.04285168076791));
#10471=CARTESIAN_POINT('Ctrl Pts',(-129.270292978784,21.4999999999999,2.03896089378841));
#10472=CARTESIAN_POINT('Ctrl Pts',(-129.3,21.4999999999999,2.03896089378841));
#10473=CARTESIAN_POINT('Origin',(-141.,21.1999999999999,15.7));
#10474=CARTESIAN_POINT('',(-141.,21.1999999999999,16.));
#10475=CARTESIAN_POINT('',(-141.,21.4999999999999,15.7));
#10476=CARTESIAN_POINT('Origin',(-129.3,-15.,15.7));
#10477=CARTESIAN_POINT('',(-129.3,-15.,16.));
#10478=CARTESIAN_POINT('',(-129.,-15.,15.7));
#10479=CARTESIAN_POINT('Origin',(-144.7,21.1999999999999,1.01948044689421));
#10480=CARTESIAN_POINT('',(-145.,21.1999999999999,2.29525996204705));
#10481=CARTESIAN_POINT('',(-145.,21.1999999999999,1.01948044689421));
#10482=CARTESIAN_POINT('',(-144.7,21.4999999999999,2.03896089378841));
#10483=CARTESIAN_POINT('',(-144.7,21.4999999999999,1.01948044689421));
#10484=CARTESIAN_POINT('Ctrl Pts',(-144.7,21.4999999999999,2.03896089378841));
#10485=CARTESIAN_POINT('Ctrl Pts',(-144.729707021216,21.4999999999999,2.03896089378841));
#10486=CARTESIAN_POINT('Ctrl Pts',(-144.758777673282,21.4955937057347,2.04285168076792));
#10487=CARTESIAN_POINT('Ctrl Pts',(-144.817440852233,21.4779567710066,2.05836227087722));
#10488=CARTESIAN_POINT('Ctrl Pts',(-144.845615509175,21.4640057619501,2.07060652861162));
#10489=CARTESIAN_POINT('Ctrl Pts',(-144.902101216584,21.4250399915451,2.10457296342855));
#10490=CARTESIAN_POINT('Ctrl Pts',(-144.927927434013,21.3982203268002,2.12780612534895));
#10491=CARTESIAN_POINT('Ctrl Pts',(-144.964853191741,21.3441129754836,2.17419410934394));
#10492=CARTESIAN_POINT('Ctrl Pts',(-144.977648024164,21.3172521646773,2.19704892779082));
#10493=CARTESIAN_POINT('Ctrl Pts',(-144.995183002517,21.2612564013421,2.24427435401479));
#10494=CARTESIAN_POINT('Ctrl Pts',(-144.99975020409,21.2318642099517,2.26885093208373));
#10495=CARTESIAN_POINT('Ctrl Pts',(-144.999996676586,21.2016304842259,2.29390907945453));
#10496=CARTESIAN_POINT('Ctrl Pts',(-145.,21.2008152808565,2.29458456963201));
#10497=CARTESIAN_POINT('Ctrl Pts',(-145.,21.1999999999999,2.29525996204705));
#10498=CARTESIAN_POINT('Origin',(-141.,-21.1999999999999,15.7));
#10499=CARTESIAN_POINT('',(-141.,-21.1999999999999,16.));
#10500=CARTESIAN_POINT('',(-141.,-21.4999999999999,15.7));
#10501=CARTESIAN_POINT('Origin',(-129.3,-21.1999999999999,1.01948044689421));
#10502=CARTESIAN_POINT('',(-129.,-21.1999999999999,2.29525996204705));
#10503=CARTESIAN_POINT('',(-129.,-21.1999999999999,1.01948044689421));
#10504=CARTESIAN_POINT('',(-129.3,-21.4999999999999,2.03896089378841));
#10505=CARTESIAN_POINT('',(-129.3,-21.4999999999999,1.01948044689421));
#10506=CARTESIAN_POINT('Ctrl Pts',(-129.3,-21.4999999999999,2.03896089378841));
#10507=CARTESIAN_POINT('Ctrl Pts',(-129.270292978784,-21.4999999999999,
2.03896089378841));
#10508=CARTESIAN_POINT('Ctrl Pts',(-129.241222326718,-21.4955937057347,
2.04285168076791));
#10509=CARTESIAN_POINT('Ctrl Pts',(-129.182559147767,-21.4779567710066,
2.05836227087723));
#10510=CARTESIAN_POINT('Ctrl Pts',(-129.154384490824,-21.4640057619501,
2.07060652861162));
#10511=CARTESIAN_POINT('Ctrl Pts',(-129.097898783416,-21.4250399915451,
2.10457296342855));
#10512=CARTESIAN_POINT('Ctrl Pts',(-129.072072565987,-21.3982203268002,
2.12780612534895));
#10513=CARTESIAN_POINT('Ctrl Pts',(-129.035146808259,-21.3441129754836,
2.17419410934393));
#10514=CARTESIAN_POINT('Ctrl Pts',(-129.022351975836,-21.3172521646773,
2.19704892779082));
#10515=CARTESIAN_POINT('Ctrl Pts',(-129.004816997483,-21.2612564013421,
2.24427435401479));
#10516=CARTESIAN_POINT('Ctrl Pts',(-129.000249795909,-21.2318642099517,
2.26885093208373));
#10517=CARTESIAN_POINT('Ctrl Pts',(-129.000003323414,-21.2016304842259,
2.29390907945453));
#10518=CARTESIAN_POINT('Ctrl Pts',(-129.,-21.2008152808565,2.29458456963201));
#10519=CARTESIAN_POINT('Ctrl Pts',(-129.,-21.1999999999999,2.29525996204705));
#10520=CARTESIAN_POINT('Origin',(-129.3,21.9999999999999,-1.92966607280848));
#10521=CARTESIAN_POINT('Origin',(-129.3,21.9999999999999,-1.92966607280848));
#10522=CARTESIAN_POINT('Origin',(-129.,21.9999999999999,-1.92966607280848));
#10523=CARTESIAN_POINT('Origin',(-144.7,-21.1999999999999,1.01948044689421));
#10524=CARTESIAN_POINT('',(-144.7,-21.4999999999999,2.03896089378841));
#10525=CARTESIAN_POINT('',(-144.7,-21.4999999999999,1.01948044689421));
#10526=CARTESIAN_POINT('',(-145.,-21.1999999999999,2.29525996204705));
#10527=CARTESIAN_POINT('',(-145.,-21.1999999999999,1.01948044689421));
#10528=CARTESIAN_POINT('Ctrl Pts',(-145.,-21.1999999999999,2.29525996204705));
#10529=CARTESIAN_POINT('Ctrl Pts',(-145.,-21.2008152808404,2.29458456964534));
#10530=CARTESIAN_POINT('Ctrl Pts',(-144.999996676585,-21.2016304842412,
2.29390907943587));
#10531=CARTESIAN_POINT('Ctrl Pts',(-144.999750204092,-21.2318642097648,
2.26885093228761));
#10532=CARTESIAN_POINT('Ctrl Pts',(-144.995183002528,-21.2612564013074,
2.24427435404393));
#10533=CARTESIAN_POINT('Ctrl Pts',(-144.977648024164,-21.3172521646786,
2.19704892778962));
#10534=CARTESIAN_POINT('Ctrl Pts',(-144.964853191741,-21.3441129754842,
2.17419410934337));
#10535=CARTESIAN_POINT('Ctrl Pts',(-144.927927434013,-21.3982203268002,
2.12780612534895));
#10536=CARTESIAN_POINT('Ctrl Pts',(-144.902101216584,-21.4250399915451,
2.10457296342854));
#10537=CARTESIAN_POINT('Ctrl Pts',(-144.845615509175,-21.4640057619501,
2.07060652861161));
#10538=CARTESIAN_POINT('Ctrl Pts',(-144.817440852233,-21.4779567710066,
2.05836227087722));
#10539=CARTESIAN_POINT('Ctrl Pts',(-144.758777673282,-21.4955937057347,
2.04285168076792));
#10540=CARTESIAN_POINT('Ctrl Pts',(-144.729707021216,-21.4999999999999,
2.03896089378841));
#10541=CARTESIAN_POINT('Ctrl Pts',(-144.7,-21.4999999999999,2.03896089378841));
#10542=CARTESIAN_POINT('Origin',(-144.7,21.9999999999999,-1.92966607280848));
#10543=CARTESIAN_POINT('Origin',(-145.,21.9999999999999,-1.92966607280848));
#10544=CARTESIAN_POINT('Origin',(-144.7,21.9999999999999,-1.92966607280848));
#10545=CARTESIAN_POINT('Origin',(-129.3,-21.9999999999999,-1.92966607280848));
#10546=CARTESIAN_POINT('Origin',(-129.,-21.9999999999999,-1.92966607280848));
#10547=CARTESIAN_POINT('Origin',(-129.3,-21.9999999999999,-1.92966607280848));
#10548=CARTESIAN_POINT('Origin',(-144.7,-21.9999999999999,-1.92966607280848));
#10549=CARTESIAN_POINT('Origin',(-144.7,-21.9999999999999,-1.92966607280848));
#10550=CARTESIAN_POINT('Origin',(-145.,-21.9999999999999,-1.92966607280848));
#10551=CARTESIAN_POINT('Origin',(-144.7,15.,15.7));
#10552=CARTESIAN_POINT('',(-144.7,15.,16.));
#10553=CARTESIAN_POINT('',(-145.,15.,15.7));
#10554=CARTESIAN_POINT('Origin',(-141.,-22.7999999999999,15.7));
#10555=CARTESIAN_POINT('',(-141.,-22.7999999999999,16.));
#10556=CARTESIAN_POINT('',(-141.,-22.4999999999999,15.7));
#10557=CARTESIAN_POINT('Origin',(-129.3,-15.,15.7));
#10558=CARTESIAN_POINT('',(-129.3,-15.,16.));
#10559=CARTESIAN_POINT('',(-129.,-15.,15.7));
#10560=CARTESIAN_POINT('Origin',(-141.,-29.7,15.7));
#10561=CARTESIAN_POINT('',(-141.,-29.7,16.));
#10562=CARTESIAN_POINT('',(-141.,-30.,15.7));
#10563=CARTESIAN_POINT('Origin',(-129.3,2.5,-10.3));
#10564=CARTESIAN_POINT('',(-129.,2.5,-10.3));
#10565=CARTESIAN_POINT('Origin',(-133.,30.3,-9.7));
#10566=CARTESIAN_POINT('',(-133.,30.,-9.7));
#10567=CARTESIAN_POINT('Origin',(-144.7,32.5,-10.3));
#10568=CARTESIAN_POINT('',(-145.,32.5,-10.3));
#10569=CARTESIAN_POINT('Origin',(-141.,-30.3,-9.7));
#10570=CARTESIAN_POINT('',(-141.,-30.,-9.7));
#10571=CARTESIAN_POINT('Origin',(-129.3,-32.5,-10.3));
#10572=CARTESIAN_POINT('',(-129.,-32.5,-10.3));
#10573=CARTESIAN_POINT('Origin',(-129.3,39.7,-8.));
#10574=CARTESIAN_POINT('',(-129.,39.7,-8.));
#10575=CARTESIAN_POINT('',(-129.3,40.,-8.));
#10576=CARTESIAN_POINT('Origin',(-144.7,-2.5,-10.3));
#10577=CARTESIAN_POINT('',(-145.,-2.5,-10.3));
#10578=CARTESIAN_POINT('Origin',(-144.7,39.7,-8.));
#10579=CARTESIAN_POINT('',(-144.7,40.,-8.));
#10580=CARTESIAN_POINT('',(-145.,39.7,-8.));
#10581=CARTESIAN_POINT('Origin',(-141.,-39.7,-10.3));
#10582=CARTESIAN_POINT('',(-141.,-40.,-10.3));
#10583=CARTESIAN_POINT('Origin',(-141.,-39.7,-15.7));
#10584=CARTESIAN_POINT('',(-141.,-39.7,-16.));
#10585=CARTESIAN_POINT('',(-141.,-40.,-15.7));
#10586=CARTESIAN_POINT('Origin',(-145.,21.4999999999999,2.03896089378841));
#10587=CARTESIAN_POINT('',(-145.,21.4999999999999,2.03896089378841));
#10588=CARTESIAN_POINT('Origin',(-145.,21.9999999999999,-1.92966607280848));
#10589=CARTESIAN_POINT('',(-145.,22.4999999999999,2.03896089378841));
#10590=CARTESIAN_POINT('Origin',(-145.,-21.9999999999999,-1.92966607280848));
#10591=CARTESIAN_POINT('',(-145.,-21.4999999999999,2.03896089378841));
#10592=CARTESIAN_POINT('',(-145.,-22.4999999999999,2.03896089378841));
#10593=CARTESIAN_POINT('Origin',(-145.,-21.4999999999999,2.03896089378841));
#10594=CARTESIAN_POINT('Origin',(-137.,-4.44089209850063E-15,-16.));
#10595=CARTESIAN_POINT('Origin',(-145.,-40.,-16.));
#10596=CARTESIAN_POINT('Origin',(-145.,40.,-16.));
#10597=CARTESIAN_POINT('Origin',(-145.,-30.,0.));
#10598=CARTESIAN_POINT('Origin',(-137.,-4.44089209850063E-15,16.));
#10599=CARTESIAN_POINT('Origin',(-129.,30.,0.));
#10600=CARTESIAN_POINT('Origin',(-137.,-4.44089209850063E-15,16.));
#10601=CARTESIAN_POINT('Origin',(-145.,30.,0.));
#10602=CARTESIAN_POINT('Origin',(-137.,-4.44089209850063E-15,16.));
#10603=CARTESIAN_POINT('Origin',(-129.,-30.,0.));
#10604=CARTESIAN_POINT('Origin',(-145.,22.4999999999999,16.));
#10605=CARTESIAN_POINT('Origin',(-145.,-22.4999999999999,16.));
#10606=CARTESIAN_POINT('',(0.,0.,0.));
#10607=CARTESIAN_POINT('',(0.,0.,0.));
#10608=CARTESIAN_POINT('',(0.,0.,0.));
#10609=CARTESIAN_POINT('',(0.,0.,0.));
#10610=CARTESIAN_POINT('',(0.,0.,0.));
#10611=CARTESIAN_POINT('',(0.,0.,0.));
#10612=CARTESIAN_POINT('',(0.,0.,0.));
#10613=CARTESIAN_POINT('',(0.,0.,0.));
#10614=CARTESIAN_POINT('',(0.,0.,0.));
#10615=CARTESIAN_POINT('',(0.,0.,0.));
#10616=UNCERTAINTY_MEASURE_WITH_UNIT(LENGTH_MEASURE(0.01),#10640,
'DISTANCE_ACCURACY_VALUE',
'Maximum model space distance between geometric entities at asserted c
onnectivities');
#10617=UNCERTAINTY_MEASURE_WITH_UNIT(LENGTH_MEASURE(0.01),#10640,
'DISTANCE_ACCURACY_VALUE',
'Maximum model space distance between geometric entities at asserted c
onnectivities');
#10618=UNCERTAINTY_MEASURE_WITH_UNIT(LENGTH_MEASURE(0.01),#10640,
'DISTANCE_ACCURACY_VALUE',
'Maximum model space distance between geometric entities at asserted c
onnectivities');
#10619=UNCERTAINTY_MEASURE_WITH_UNIT(LENGTH_MEASURE(0.01),#10640,
'DISTANCE_ACCURACY_VALUE',
'Maximum model space distance between geometric entities at asserted c
onnectivities');
#10620=UNCERTAINTY_MEASURE_WITH_UNIT(LENGTH_MEASURE(0.01),#10640,
'DISTANCE_ACCURACY_VALUE',
'Maximum model space distance between geometric entities at asserted c
onnectivities');
#10621=UNCERTAINTY_MEASURE_WITH_UNIT(LENGTH_MEASURE(0.01),#10640,
'DISTANCE_ACCURACY_VALUE',
'Maximum model space distance between geometric entities at asserted c
onnectivities');
#10622=UNCERTAINTY_MEASURE_WITH_UNIT(LENGTH_MEASURE(0.01),#10640,
'DISTANCE_ACCURACY_VALUE',
'Maximum model space distance between geometric entities at asserted c
onnectivities');
#10623=UNCERTAINTY_MEASURE_WITH_UNIT(LENGTH_MEASURE(0.01),#10640,
'DISTANCE_ACCURACY_VALUE',
'Maximum model space distance between geometric entities at asserted c
onnectivities');
#10624=UNCERTAINTY_MEASURE_WITH_UNIT(LENGTH_MEASURE(0.01),#10640,
'DISTANCE_ACCURACY_VALUE',
'Maximum model space distance between geometric entities at asserted c
onnectivities');
#10625=UNCERTAINTY_MEASURE_WITH_UNIT(LENGTH_MEASURE(0.01),#10640,
'DISTANCE_ACCURACY_VALUE',
'Maximum model space distance between geometric entities at asserted c
onnectivities');
#10626=UNCERTAINTY_MEASURE_WITH_UNIT(LENGTH_MEASURE(0.01),#10640,
'DISTANCE_ACCURACY_VALUE',
'Maximum model space distance between geometric entities at asserted c
onnectivities');
#10627=UNCERTAINTY_MEASURE_WITH_UNIT(LENGTH_MEASURE(0.01),#10640,
'DISTANCE_ACCURACY_VALUE',
'Maximum model space distance between geometric entities at asserted c
onnectivities');
#10628=(
GEOMETRIC_REPRESENTATION_CONTEXT(3)
GLOBAL_UNCERTAINTY_ASSIGNED_CONTEXT((#10616))
GLOBAL_UNIT_ASSIGNED_CONTEXT((#10640,#10642,#10643))
REPRESENTATION_CONTEXT('','3D')
);
#10629=(
GEOMETRIC_REPRESENTATION_CONTEXT(3)
GLOBAL_UNCERTAINTY_ASSIGNED_CONTEXT((#10617))
GLOBAL_UNIT_ASSIGNED_CONTEXT((#10640,#10642,#10643))
REPRESENTATION_CONTEXT('','3D')
);
#10630=(
GEOMETRIC_REPRESENTATION_CONTEXT(3)
GLOBAL_UNCERTAINTY_ASSIGNED_CONTEXT((#10618))
GLOBAL_UNIT_ASSIGNED_CONTEXT((#10640,#10642,#10643))
REPRESENTATION_CONTEXT('','3D')
);
#10631=(
GEOMETRIC_REPRESENTATION_CONTEXT(3)
GLOBAL_UNCERTAINTY_ASSIGNED_CONTEXT((#10619))
GLOBAL_UNIT_ASSIGNED_CONTEXT((#10640,#10642,#10643))
REPRESENTATION_CONTEXT('','3D')
);
#10632=(
GEOMETRIC_REPRESENTATION_CONTEXT(3)
GLOBAL_UNCERTAINTY_ASSIGNED_CONTEXT((#10620))
GLOBAL_UNIT_ASSIGNED_CONTEXT((#10640,#10642,#10643))
REPRESENTATION_CONTEXT('','3D')
);
#10633=(
GEOMETRIC_REPRESENTATION_CONTEXT(3)
GLOBAL_UNCERTAINTY_ASSIGNED_CONTEXT((#10621))
GLOBAL_UNIT_ASSIGNED_CONTEXT((#10640,#10642,#10643))
REPRESENTATION_CONTEXT('','3D')
);
#10634=(
GEOMETRIC_REPRESENTATION_CONTEXT(3)
GLOBAL_UNCERTAINTY_ASSIGNED_CONTEXT((#10622))
GLOBAL_UNIT_ASSIGNED_CONTEXT((#10640,#10642,#10643))
REPRESENTATION_CONTEXT('','3D')
);
#10635=(
GEOMETRIC_REPRESENTATION_CONTEXT(3)
GLOBAL_UNCERTAINTY_ASSIGNED_CONTEXT((#10623))
GLOBAL_UNIT_ASSIGNED_CONTEXT((#10640,#10642,#10643))
REPRESENTATION_CONTEXT('','3D')
);
#10636=(
GEOMETRIC_REPRESENTATION_CONTEXT(3)
GLOBAL_UNCERTAINTY_ASSIGNED_CONTEXT((#10624))
GLOBAL_UNIT_ASSIGNED_CONTEXT((#10640,#10642,#10643))
REPRESENTATION_CONTEXT('','3D')
);
#10637=(
GEOMETRIC_REPRESENTATION_CONTEXT(3)
GLOBAL_UNCERTAINTY_ASSIGNED_CONTEXT((#10625))
GLOBAL_UNIT_ASSIGNED_CONTEXT((#10640,#10642,#10643))
REPRESENTATION_CONTEXT('','3D')
);
#10638=(
GEOMETRIC_REPRESENTATION_CONTEXT(3)
GLOBAL_UNCERTAINTY_ASSIGNED_CONTEXT((#10626))
GLOBAL_UNIT_ASSIGNED_CONTEXT((#10640,#10642,#10643))
REPRESENTATION_CONTEXT('','3D')
);
#10639=(
GEOMETRIC_REPRESENTATION_CONTEXT(3)
GLOBAL_UNCERTAINTY_ASSIGNED_CONTEXT((#10627))
GLOBAL_UNIT_ASSIGNED_CONTEXT((#10640,#10642,#10643))
REPRESENTATION_CONTEXT('','3D')
);
#10640=(
LENGTH_UNIT()
NAMED_UNIT(*)
SI_UNIT(.MILLI.,.METRE.)
);
#10641=(
LENGTH_UNIT()
NAMED_UNIT(*)
SI_UNIT($,.METRE.)
);
#10642=(
NAMED_UNIT(*)
PLANE_ANGLE_UNIT()
SI_UNIT($,.RADIAN.)
);
#10643=(
NAMED_UNIT(*)
SI_UNIT($,.STERADIAN.)
SOLID_ANGLE_UNIT()
);
#10644=SHAPE_DEFINITION_REPRESENTATION(#10655,#10676);
#10645=SHAPE_DEFINITION_REPRESENTATION(#10656,#10677);
#10646=SHAPE_DEFINITION_REPRESENTATION(#10657,#10678);
#10647=SHAPE_DEFINITION_REPRESENTATION(#10658,#10679);
#10648=SHAPE_DEFINITION_REPRESENTATION(#10659,#10680);
#10649=SHAPE_DEFINITION_REPRESENTATION(#10660,#10681);
#10650=SHAPE_DEFINITION_REPRESENTATION(#10661,#10682);
#10651=SHAPE_DEFINITION_REPRESENTATION(#10662,#10683);
#10652=SHAPE_DEFINITION_REPRESENTATION(#10663,#10684);
#10653=SHAPE_DEFINITION_REPRESENTATION(#10664,#10685);
#10654=SHAPE_DEFINITION_REPRESENTATION(#10665,#10686);
#10655=PRODUCT_DEFINITION_SHAPE('',$,#10688);
#10656=PRODUCT_DEFINITION_SHAPE('',$,#10689);
#10657=PRODUCT_DEFINITION_SHAPE('',$,#10690);
#10658=PRODUCT_DEFINITION_SHAPE('',$,#10691);
#10659=PRODUCT_DEFINITION_SHAPE('',$,#10692);
#10660=PRODUCT_DEFINITION_SHAPE('',$,#10693);
#10661=PRODUCT_DEFINITION_SHAPE('',$,#10694);
#10662=PRODUCT_DEFINITION_SHAPE('',$,#10695);
#10663=PRODUCT_DEFINITION_SHAPE('',$,#10696);
#10664=PRODUCT_DEFINITION_SHAPE('',$,#10697);
#10665=PRODUCT_DEFINITION_SHAPE('',$,#10698);
#10666=PRODUCT_DEFINITION_SHAPE($,$,#41);
#10667=PRODUCT_DEFINITION_SHAPE($,$,#42);
#10668=PRODUCT_DEFINITION_SHAPE($,$,#43);
#10669=PRODUCT_DEFINITION_SHAPE($,$,#44);
#10670=PRODUCT_DEFINITION_SHAPE($,$,#45);
#10671=PRODUCT_DEFINITION_SHAPE($,$,#46);
#10672=PRODUCT_DEFINITION_SHAPE($,$,#47);
#10673=PRODUCT_DEFINITION_SHAPE($,$,#48);
#10674=PRODUCT_DEFINITION_SHAPE($,$,#49);
#10675=PRODUCT_DEFINITION_SHAPE($,$,#50);
#10676=SHAPE_REPRESENTATION('',(#5834,#6686,#6687,#6688,#6689,#6690,#6691,
#6692,#6693,#6694,#6695),#10628);
#10677=SHAPE_REPRESENTATION('',(#5835),#10629);
#10678=SHAPE_REPRESENTATION('',(#6174),#10630);
#10679=SHAPE_REPRESENTATION('',(#6199),#10631);
#10680=SHAPE_REPRESENTATION('',(#6224),#10632);
#10681=SHAPE_REPRESENTATION('',(#6421),#10633);
#10682=SHAPE_REPRESENTATION('',(#6427),#10634);
#10683=SHAPE_REPRESENTATION('',(#6452),#10635);
#10684=SHAPE_REPRESENTATION('',(#6458),#10636);
#10685=SHAPE_REPRESENTATION('',(#6464),#10637);
#10686=SHAPE_REPRESENTATION('',(#6489),#10638);
#10687=PRODUCT_DEFINITION_CONTEXT('part definition',#10722,'design');
#10688=PRODUCT_DEFINITION('MAS-273','MAS-273',#10699,#10687);
#10689=PRODUCT_DEFINITION('Base','Base',#10700,#10687);
#10690=PRODUCT_DEFINITION('Bearing_03','Bearing_03',#10701,#10687);
#10691=PRODUCT_DEFINITION('Bearing_04','Bearing_04',#10702,#10687);
#10692=PRODUCT_DEFINITION('End_Block','End_Block',#10703,#10687);
#10693=PRODUCT_DEFINITION('Screw','Screw',#10704,#10687);
#10694=PRODUCT_DEFINITION('Bearing_02','Bearing_02',#10705,#10687);
#10695=PRODUCT_DEFINITION('Left_Rod','Left_Rod',#10706,#10687);
#10696=PRODUCT_DEFINITION('Right_Rod','Right_Rod',#10707,#10687);
#10697=PRODUCT_DEFINITION('Bearing_01','Bearing_01',#10708,#10687);
#10698=PRODUCT_DEFINITION('Front_Block','Front_Block',#10709,#10687);
#10699=PRODUCT_DEFINITION_FORMATION('',$,#10724);
#10700=PRODUCT_DEFINITION_FORMATION('',$,#10725);
#10701=PRODUCT_DEFINITION_FORMATION('',$,#10726);
#10702=PRODUCT_DEFINITION_FORMATION('',$,#10727);
#10703=PRODUCT_DEFINITION_FORMATION('',$,#10728);
#10704=PRODUCT_DEFINITION_FORMATION('',$,#10729);
#10705=PRODUCT_DEFINITION_FORMATION('',$,#10730);
#10706=PRODUCT_DEFINITION_FORMATION('',$,#10731);
#10707=PRODUCT_DEFINITION_FORMATION('',$,#10732);
#10708=PRODUCT_DEFINITION_FORMATION('',$,#10733);
#10709=PRODUCT_DEFINITION_FORMATION('',$,#10734);
#10710=PRODUCT_RELATED_PRODUCT_CATEGORY('MAS-273','MAS-273',(#10724));
#10711=PRODUCT_RELATED_PRODUCT_CATEGORY('Base','Base',(#10725));
#10712=PRODUCT_RELATED_PRODUCT_CATEGORY('Bearing_03','Bearing_03',(#10726));
#10713=PRODUCT_RELATED_PRODUCT_CATEGORY('Bearing_04','Bearing_04',(#10727));
#10714=PRODUCT_RELATED_PRODUCT_CATEGORY('End_Block','End_Block',(#10728));
#10715=PRODUCT_RELATED_PRODUCT_CATEGORY('Screw','Screw',(#10729));
#10716=PRODUCT_RELATED_PRODUCT_CATEGORY('Bearing_02','Bearing_02',(#10730));
#10717=PRODUCT_RELATED_PRODUCT_CATEGORY('Left_Rod','Left_Rod',(#10731));
#10718=PRODUCT_RELATED_PRODUCT_CATEGORY('Right_Rod','Right_Rod',(#10732));
#10719=PRODUCT_RELATED_PRODUCT_CATEGORY('Bearing_01','Bearing_01',(#10733));
#10720=PRODUCT_RELATED_PRODUCT_CATEGORY('Front_Block','Front_Block',(#10734));
#10721=APPLICATION_PROTOCOL_DEFINITION('international standard',
'automotive_design',2009,#10722);
#10722=APPLICATION_CONTEXT(
'Core Data for Automotive Mechanical Design Process');
#10723=PRODUCT_CONTEXT('part definition',#10722,'mechanical');
#10724=PRODUCT('MAS-273','MAS-273',$,(#10723));
#10725=PRODUCT('Base','Base',$,(#10723));
#10726=PRODUCT('Bearing_03','Bearing_03',$,(#10723));
#10727=PRODUCT('Bearing_04','Bearing_04',$,(#10723));
#10728=PRODUCT('End_Block','End_Block',$,(#10723));
#10729=PRODUCT('Screw','Screw',$,(#10723));
#10730=PRODUCT('Bearing_02','Bearing_02',$,(#10723));
#10731=PRODUCT('Left_Rod','Left_Rod',$,(#10723));
#10732=PRODUCT('Right_Rod','Right_Rod',$,(#10723));
#10733=PRODUCT('Bearing_01','Bearing_01',$,(#10723));
#10734=PRODUCT('Front_Block','Front_Block',$,(#10723));
#10735=PRESENTATION_STYLE_ASSIGNMENT((#10739));
#10736=PRESENTATION_STYLE_ASSIGNMENT((#10740));
#10737=PRESENTATION_STYLE_ASSIGNMENT((#10741));
#10738=PRESENTATION_STYLE_ASSIGNMENT((#10742));
#10739=SURFACE_STYLE_USAGE(.BOTH.,#10743);
#10740=SURFACE_STYLE_USAGE(.BOTH.,#10744);
#10741=SURFACE_STYLE_USAGE(.BOTH.,#10745);
#10742=SURFACE_STYLE_USAGE(.BOTH.,#10746);
#10743=SURFACE_SIDE_STYLE('',(#10747));
#10744=SURFACE_SIDE_STYLE('',(#10748));
#10745=SURFACE_SIDE_STYLE('',(#10749));
#10746=SURFACE_SIDE_STYLE('',(#10750));
#10747=SURFACE_STYLE_FILL_AREA(#10751);
#10748=SURFACE_STYLE_FILL_AREA(#10752);
#10749=SURFACE_STYLE_FILL_AREA(#10753);
#10750=SURFACE_STYLE_FILL_AREA(#10754);
#10751=FILL_AREA_STYLE('Steel - Satin',(#10755));
#10752=FILL_AREA_STYLE('Steel - Satin',(#10756));
#10753=FILL_AREA_STYLE('Steel - Satin (1)',(#10757));
#10754=FILL_AREA_STYLE('Steel - Satin (2)',(#10758));
#10755=FILL_AREA_STYLE_COLOUR('Steel - Satin',#10759);
#10756=FILL_AREA_STYLE_COLOUR('Steel - Satin',#10760);
#10757=FILL_AREA_STYLE_COLOUR('Steel - Satin (1)',#10761);
#10758=FILL_AREA_STYLE_COLOUR('Steel - Satin (2)',#10762);
#10759=COLOUR_RGB('Steel - Satin',0.627450980392157,0.627450980392157,0.627450980392157);
#10760=COLOUR_RGB('Steel - Satin',0.803921568627451,0.690196078431373,0.690196078431373);
#10761=COLOUR_RGB('Steel - Satin (1)',0.192156862745098,0.105882352941176,
0.105882352941176);
#10762=COLOUR_RGB('Steel - Satin (2)',0.858823529411765,0.858823529411765,
0.858823529411765);
#10763=COLOUR_RGB('Dark Blue',0.08,0.2,0.34);
#10764=FILL_AREA_STYLE_COLOUR('',#10763);
#10765=FILL_AREA_STYLE('',(#10764));
#10766=SURFACE_STYLE_FILL_AREA(#10765);
#10767=SURFACE_SIDE_STYLE('',(#10766));
#10768=SURFACE_STYLE_USAGE(.BOTH.,#10767);
#10769=PRESENTATION_STYLE_ASSIGNMENT((#10768));
#10770=COLOUR_RGB('Light Blue',0.38,0.62,0.78);
#10771=FILL_AREA_STYLE_COLOUR('',#10770);
#10772=FILL_AREA_STYLE('',(#10771));
#10773=SURFACE_STYLE_FILL_AREA(#10772);
#10774=SURFACE_SIDE_STYLE('',(#10773));
#10775=SURFACE_STYLE_USAGE(.BOTH.,#10774);
#10776=PRESENTATION_STYLE_ASSIGNMENT((#10775));
#10777=COLOUR_RGB('Sky Blue',0.24,0.69,0.87);
#10778=FILL_AREA_STYLE_COLOUR('',#10777);
#10779=FILL_AREA_STYLE('',(#10778));
#10780=SURFACE_STYLE_FILL_AREA(#10779);
#10781=SURFACE_SIDE_STYLE('',(#10780));
#10782=SURFACE_STYLE_USAGE(.BOTH.,#10781);
#10783=PRESENTATION_STYLE_ASSIGNMENT((#10782));
#10784=COLOUR_RGB('Grey',0.48,0.52,0.57);
#10785=FILL_AREA_STYLE_COLOUR('',#10784);
#10786=FILL_AREA_STYLE('',(#10785));
#10787=SURFACE_STYLE_FILL_AREA(#10786);
#10788=SURFACE_SIDE_STYLE('',(#10787));
#10789=SURFACE_STYLE_USAGE(.BOTH.,#10788);
#10790=PRESENTATION_STYLE_ASSIGNMENT((#10789));
#10791=COLOUR_RGB('Black',0.12,0.14,0.17);
#10792=FILL_AREA_STYLE_COLOUR('',#10791);
#10793=FILL_AREA_STYLE('',(#10792));
#10794=SURFACE_STYLE_FILL_AREA(#10793);
#10795=SURFACE_SIDE_STYLE('',(#10794));
#10796=SURFACE_STYLE_USAGE(.BOTH.,#10795);
#10797=PRESENTATION_STYLE_ASSIGNMENT((#10796));
#10798=COLOUR_RGB('Off White',0.89,0.88,0.83);
#10799=FILL_AREA_STYLE_COLOUR('',#10798);
#10800=FILL_AREA_STYLE('',(#10799));
#10801=SURFACE_STYLE_FILL_AREA(#10800);
#10802=SURFACE_SIDE_STYLE('',(#10801));
#10803=SURFACE_STYLE_USAGE(.BOTH.,#10802);
#10804=PRESENTATION_STYLE_ASSIGNMENT((#10803));
ENDSEC;
END-ISO-10303-21;
